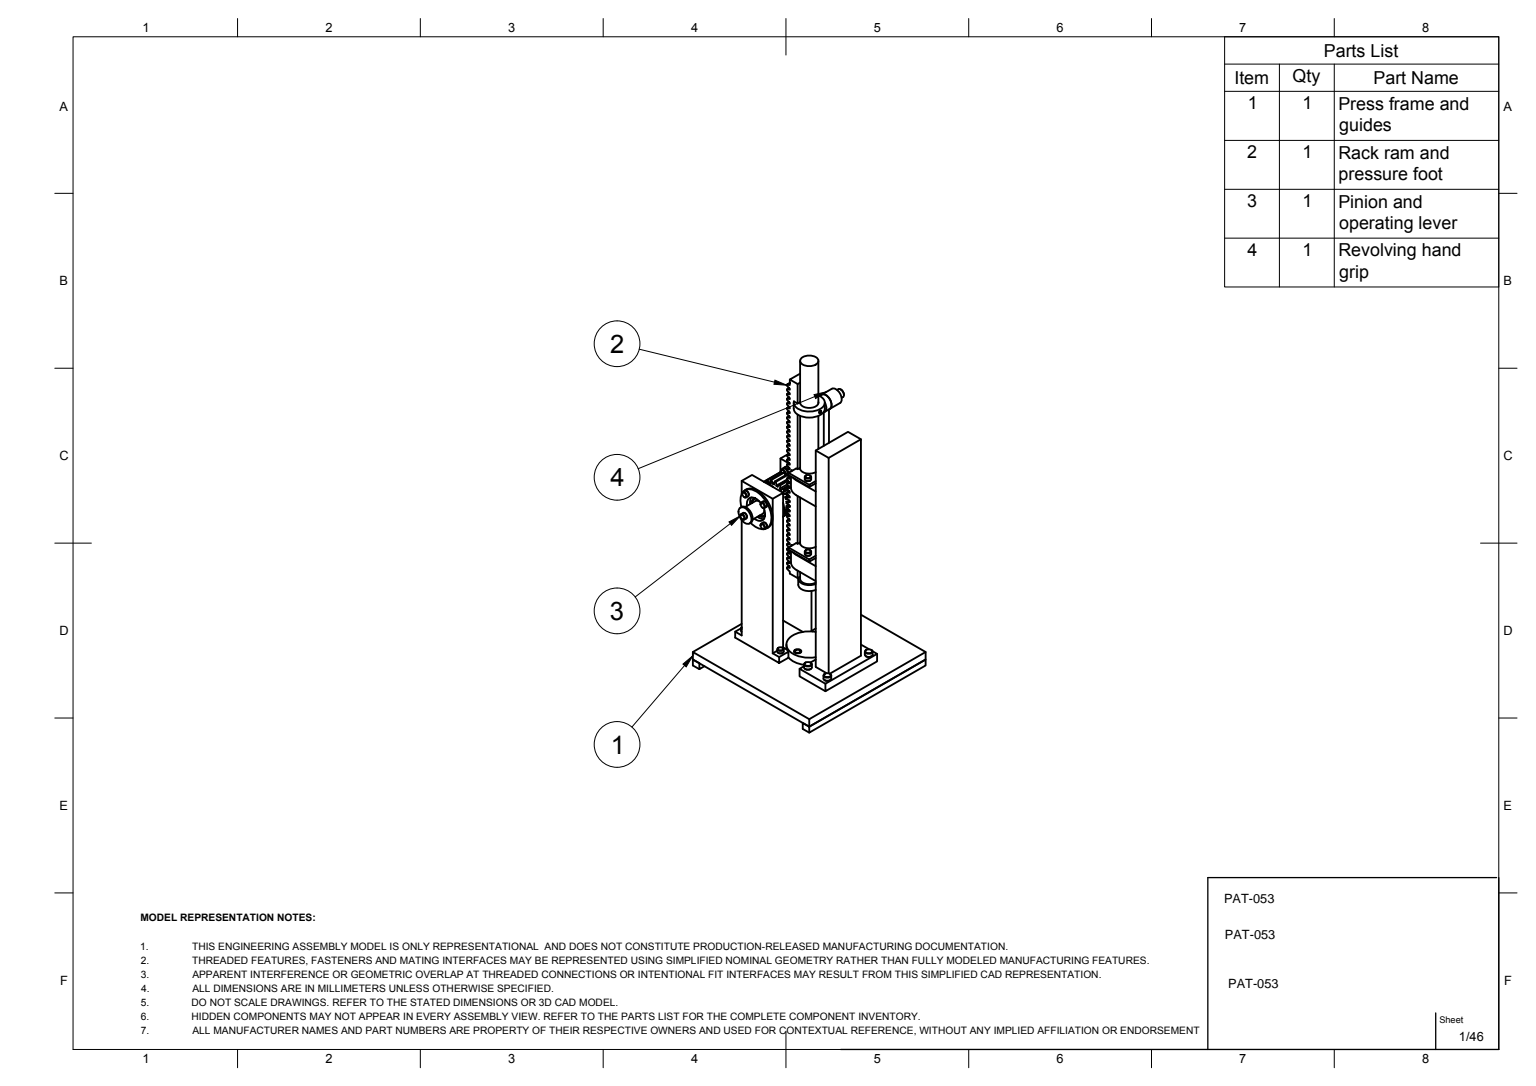
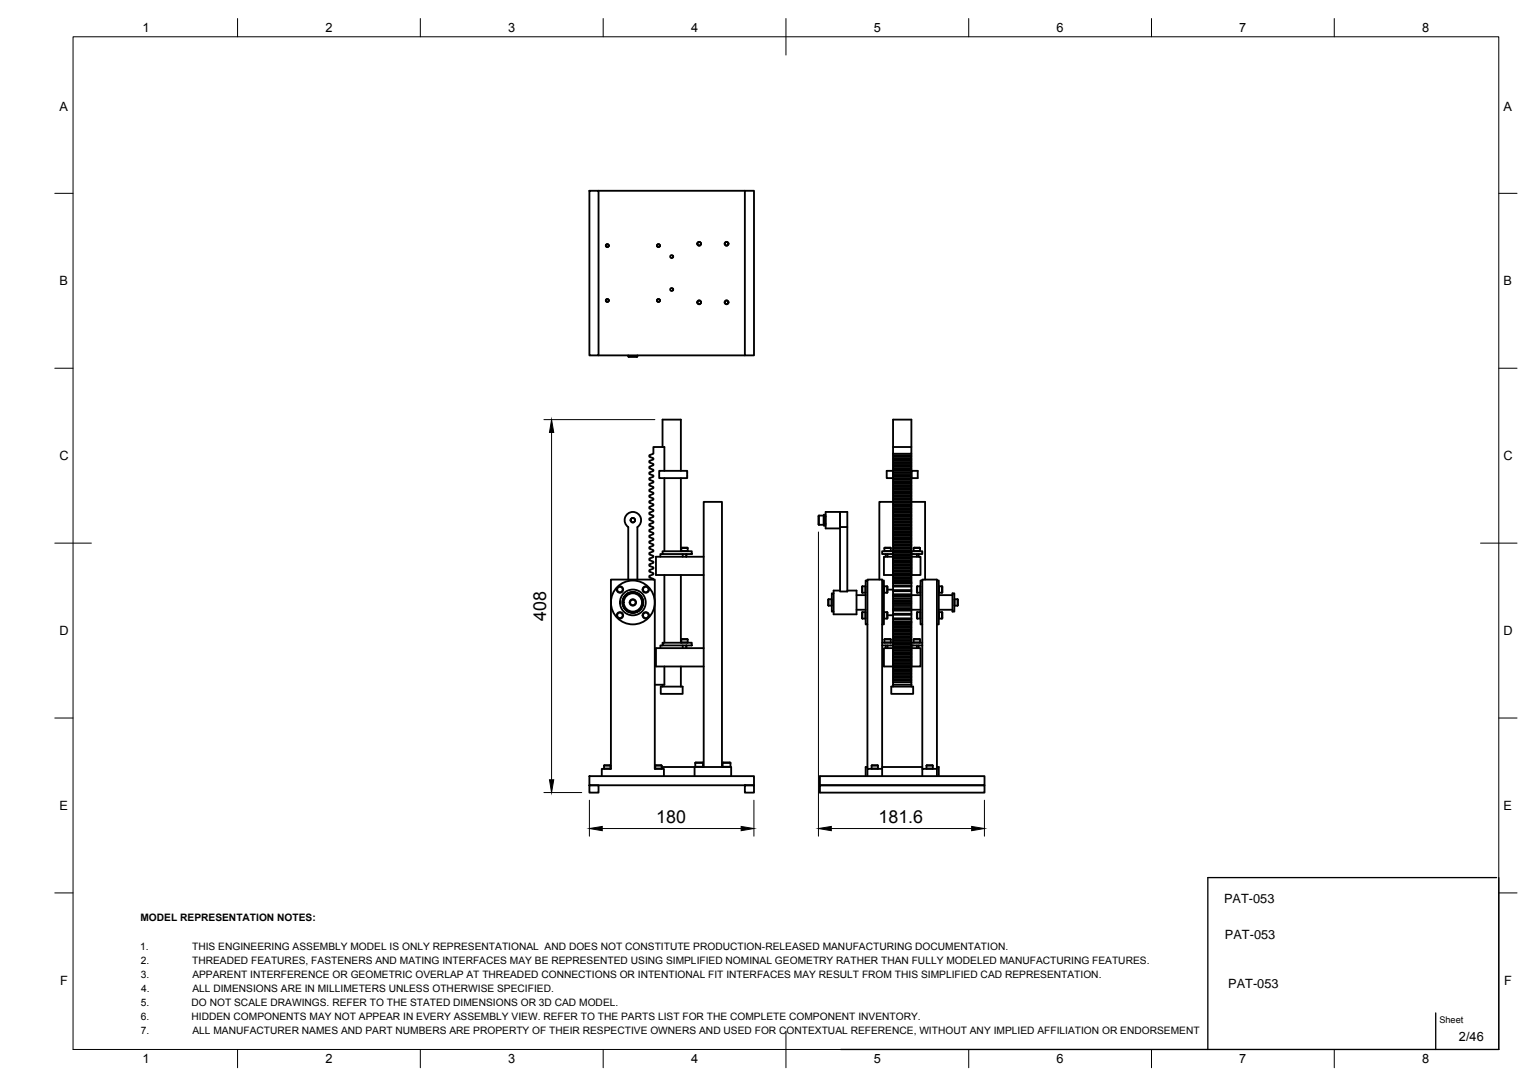
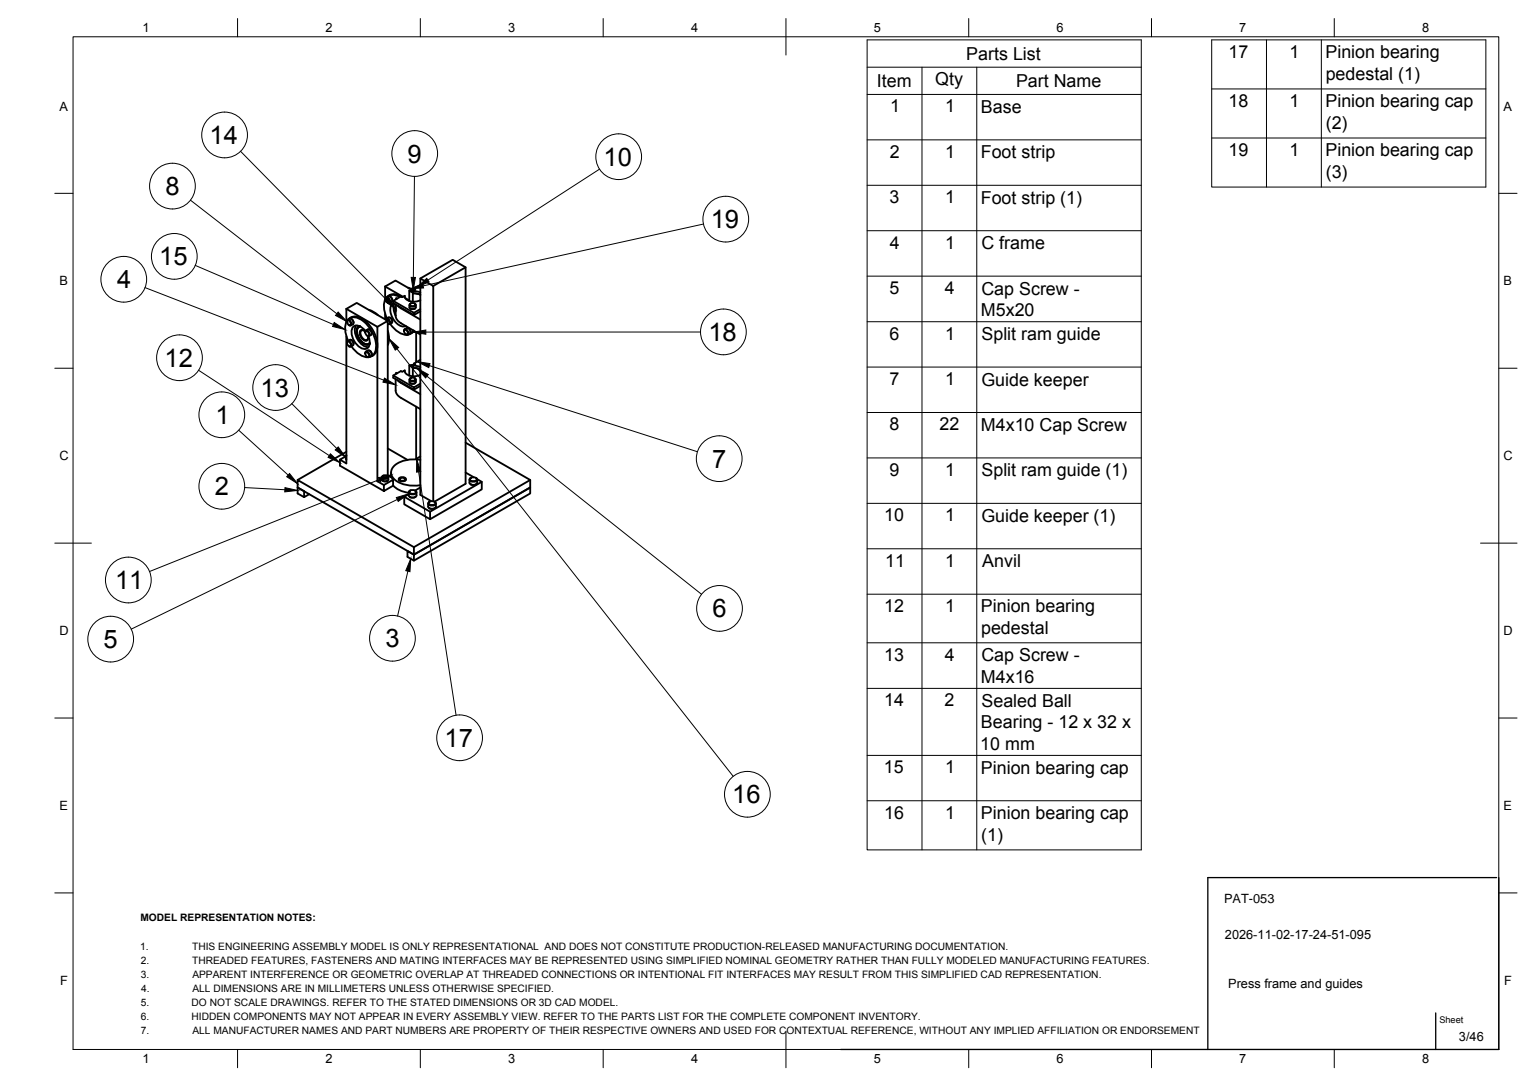
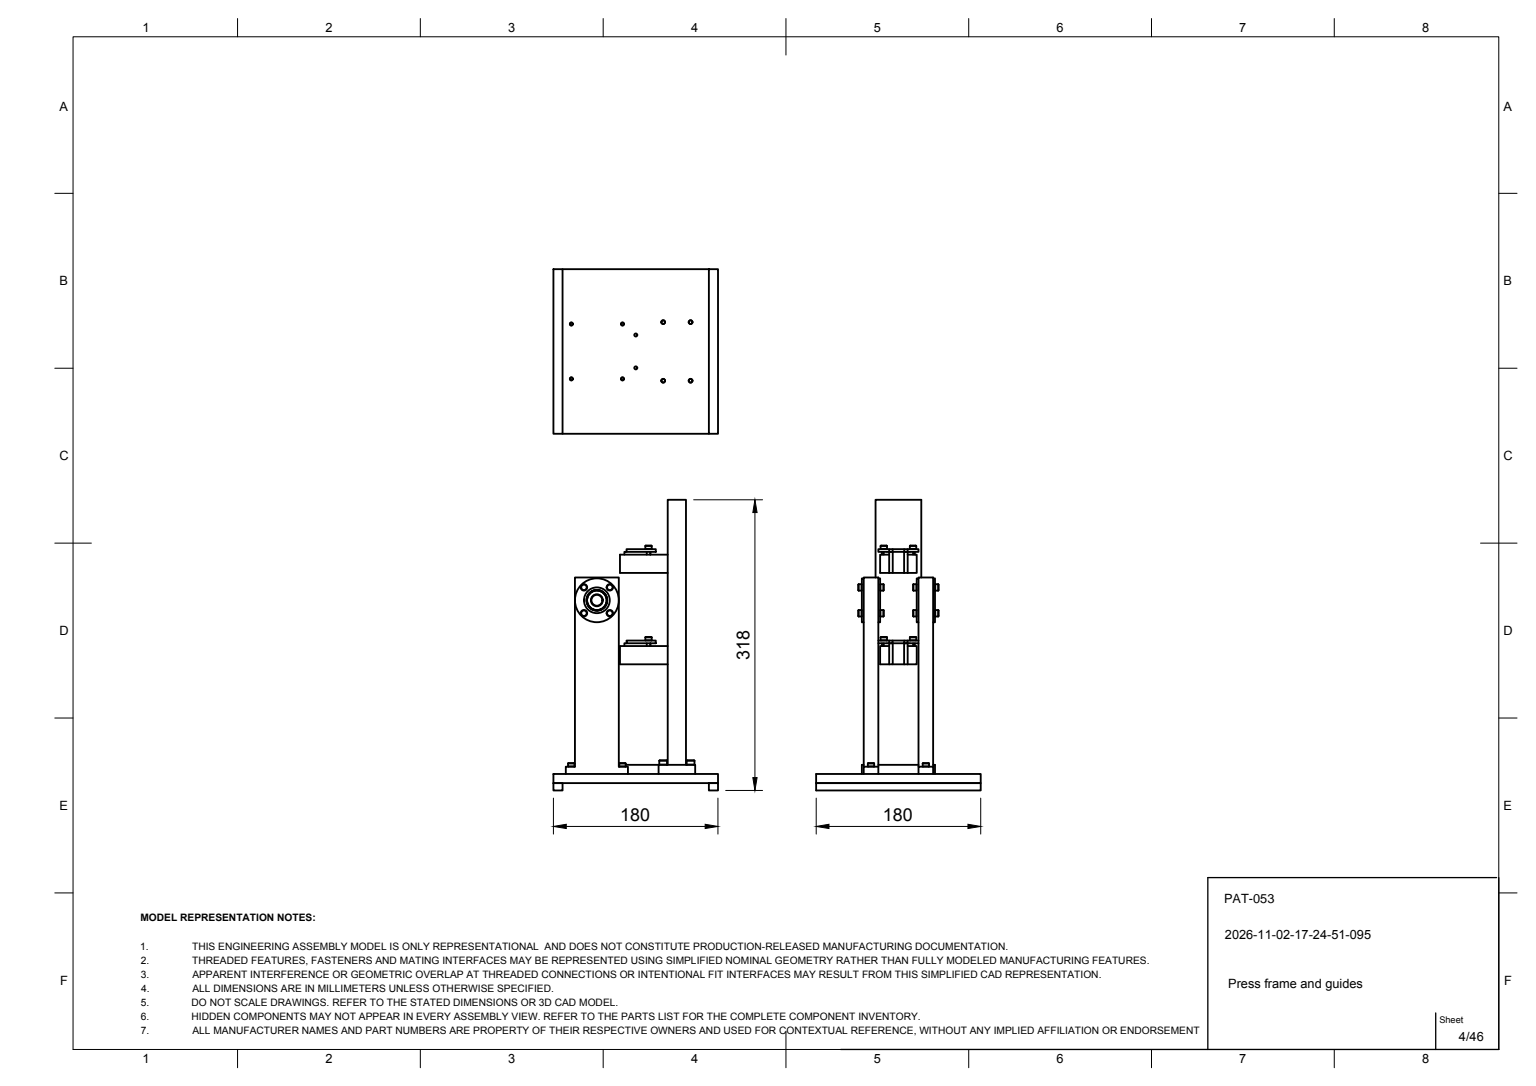
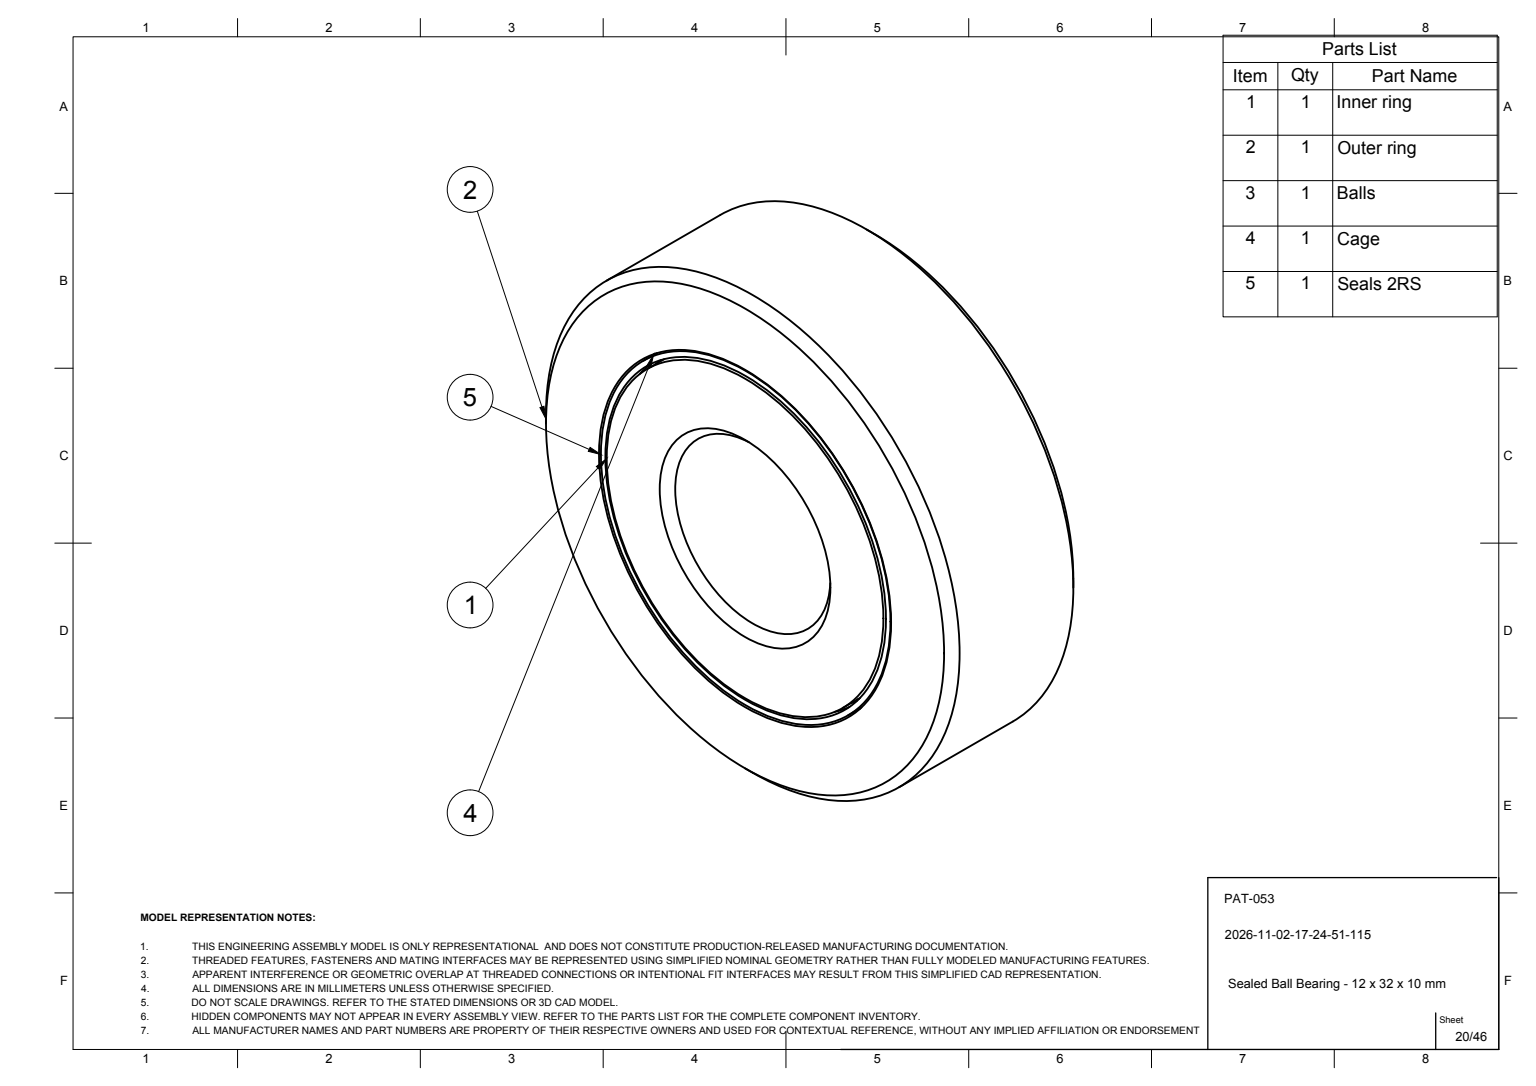
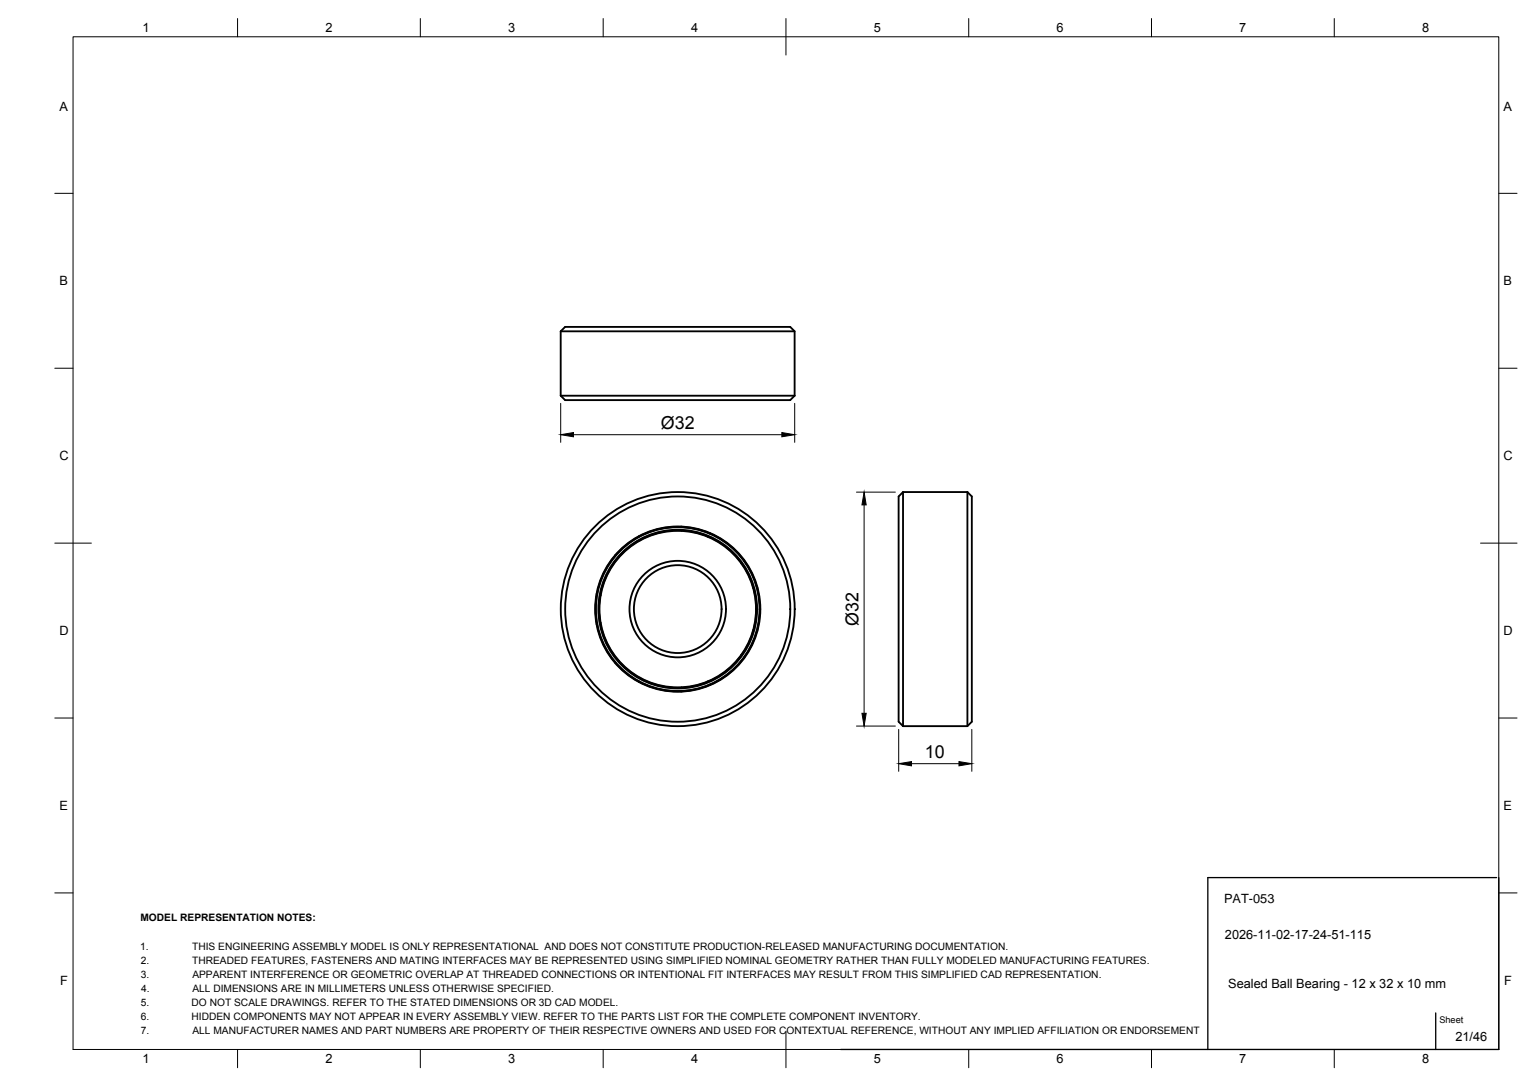
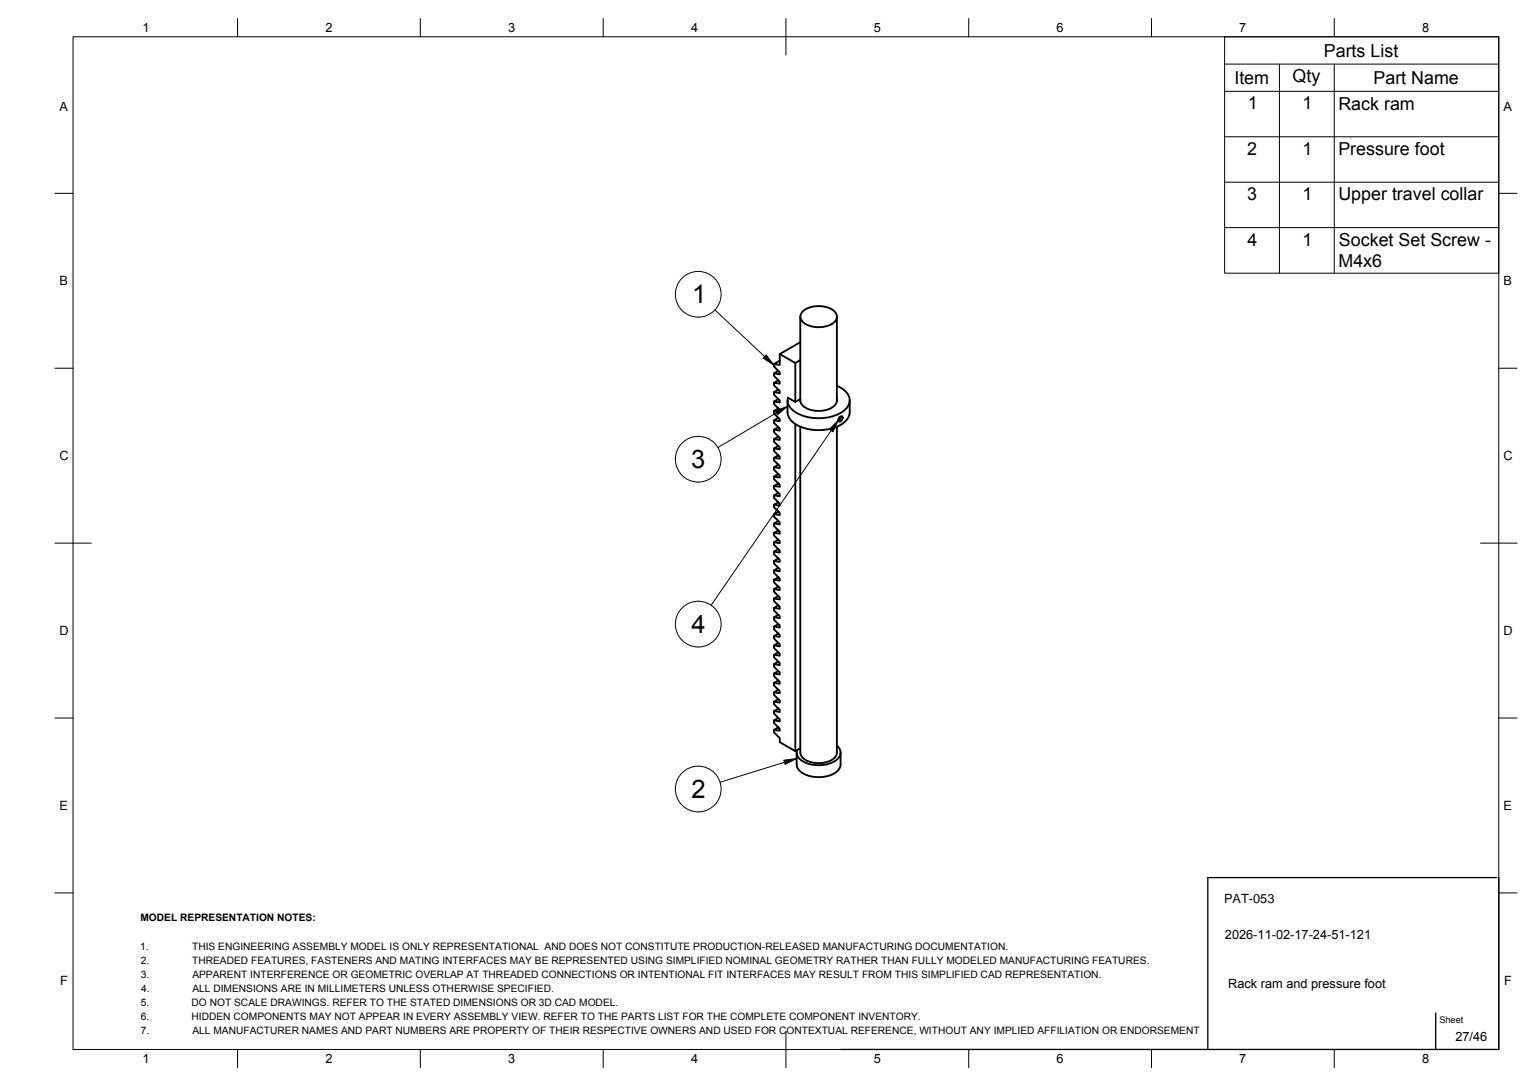
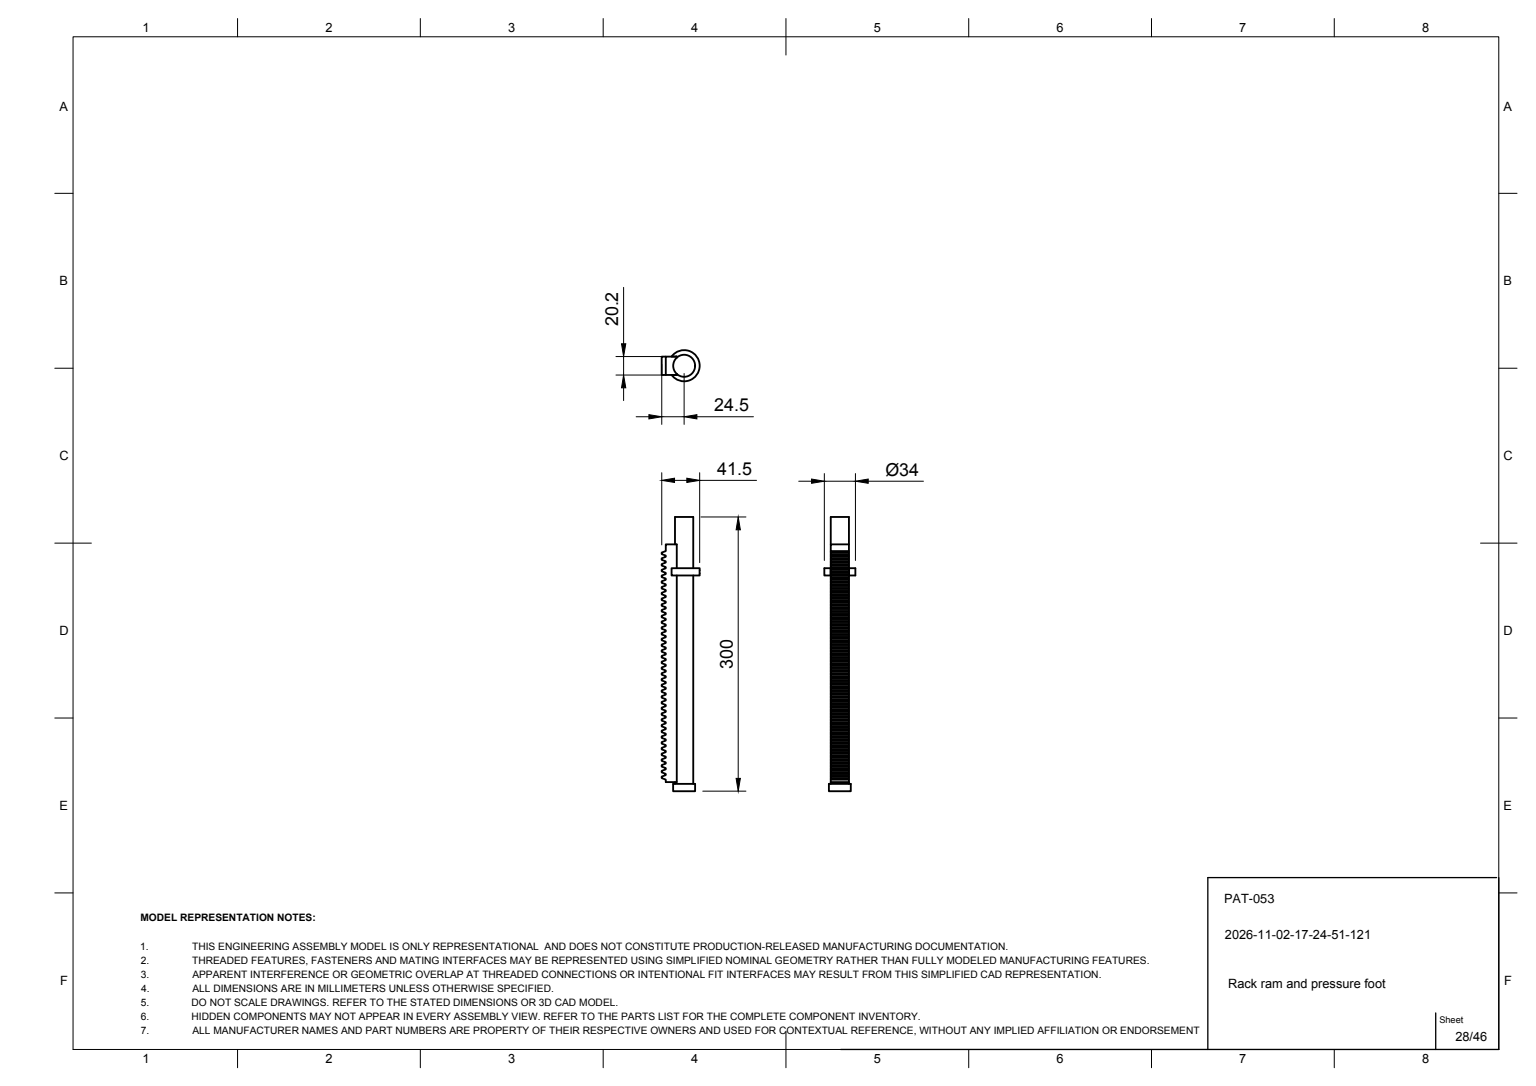
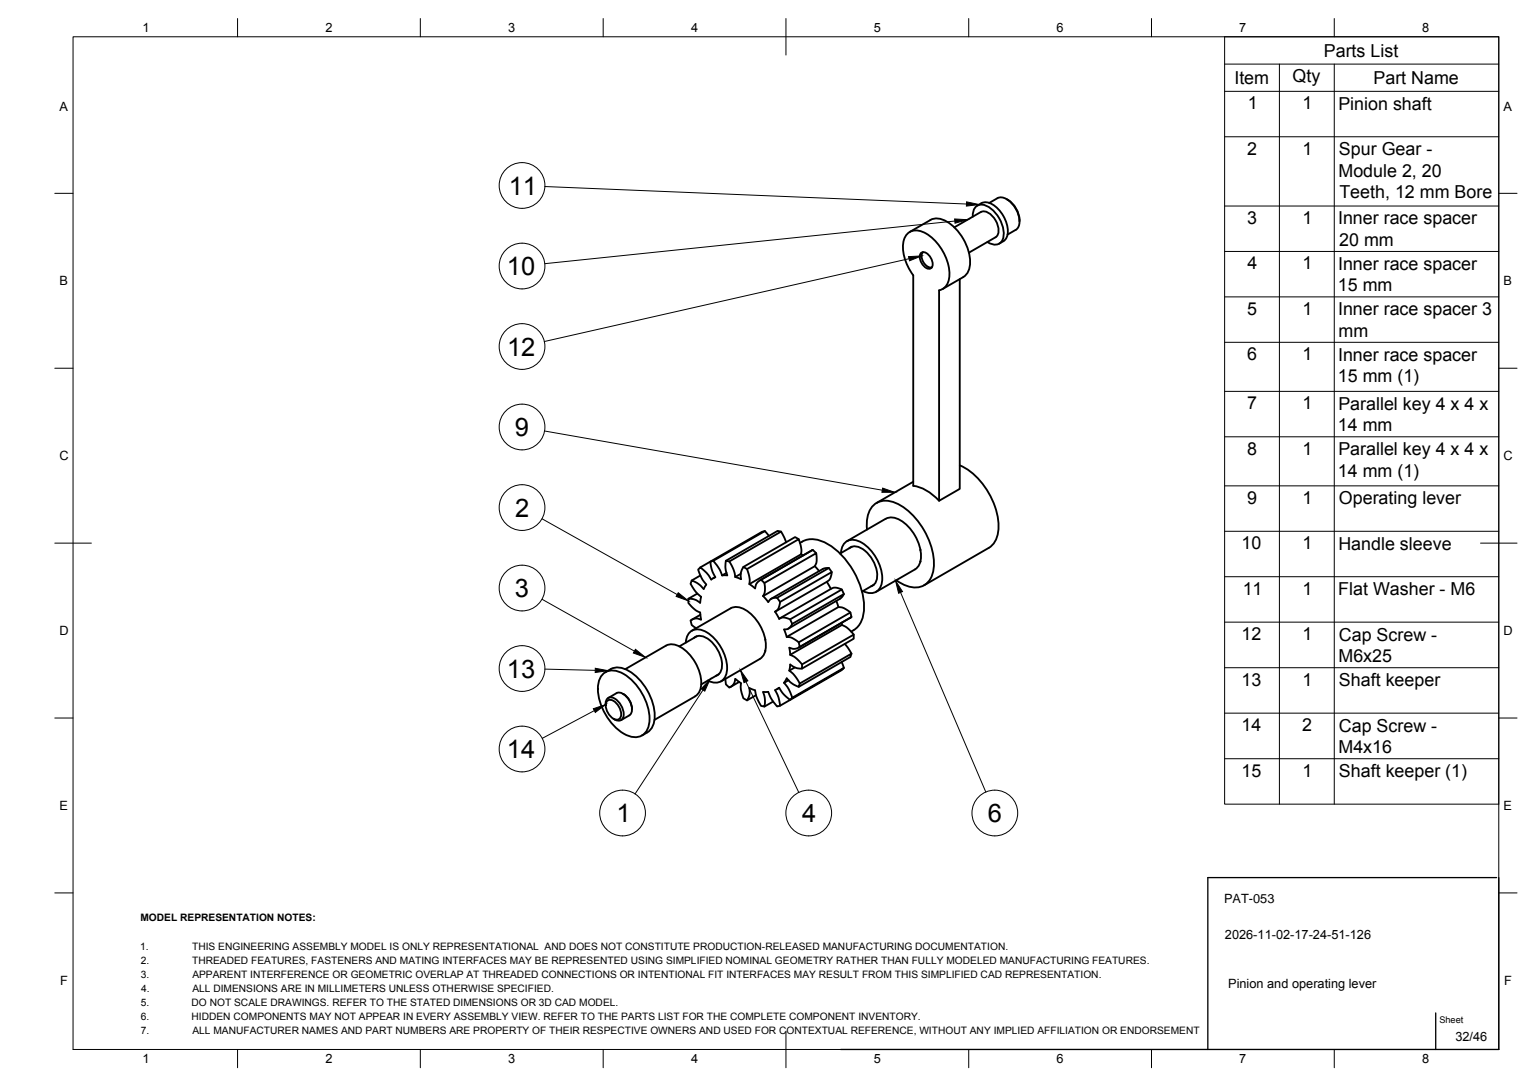
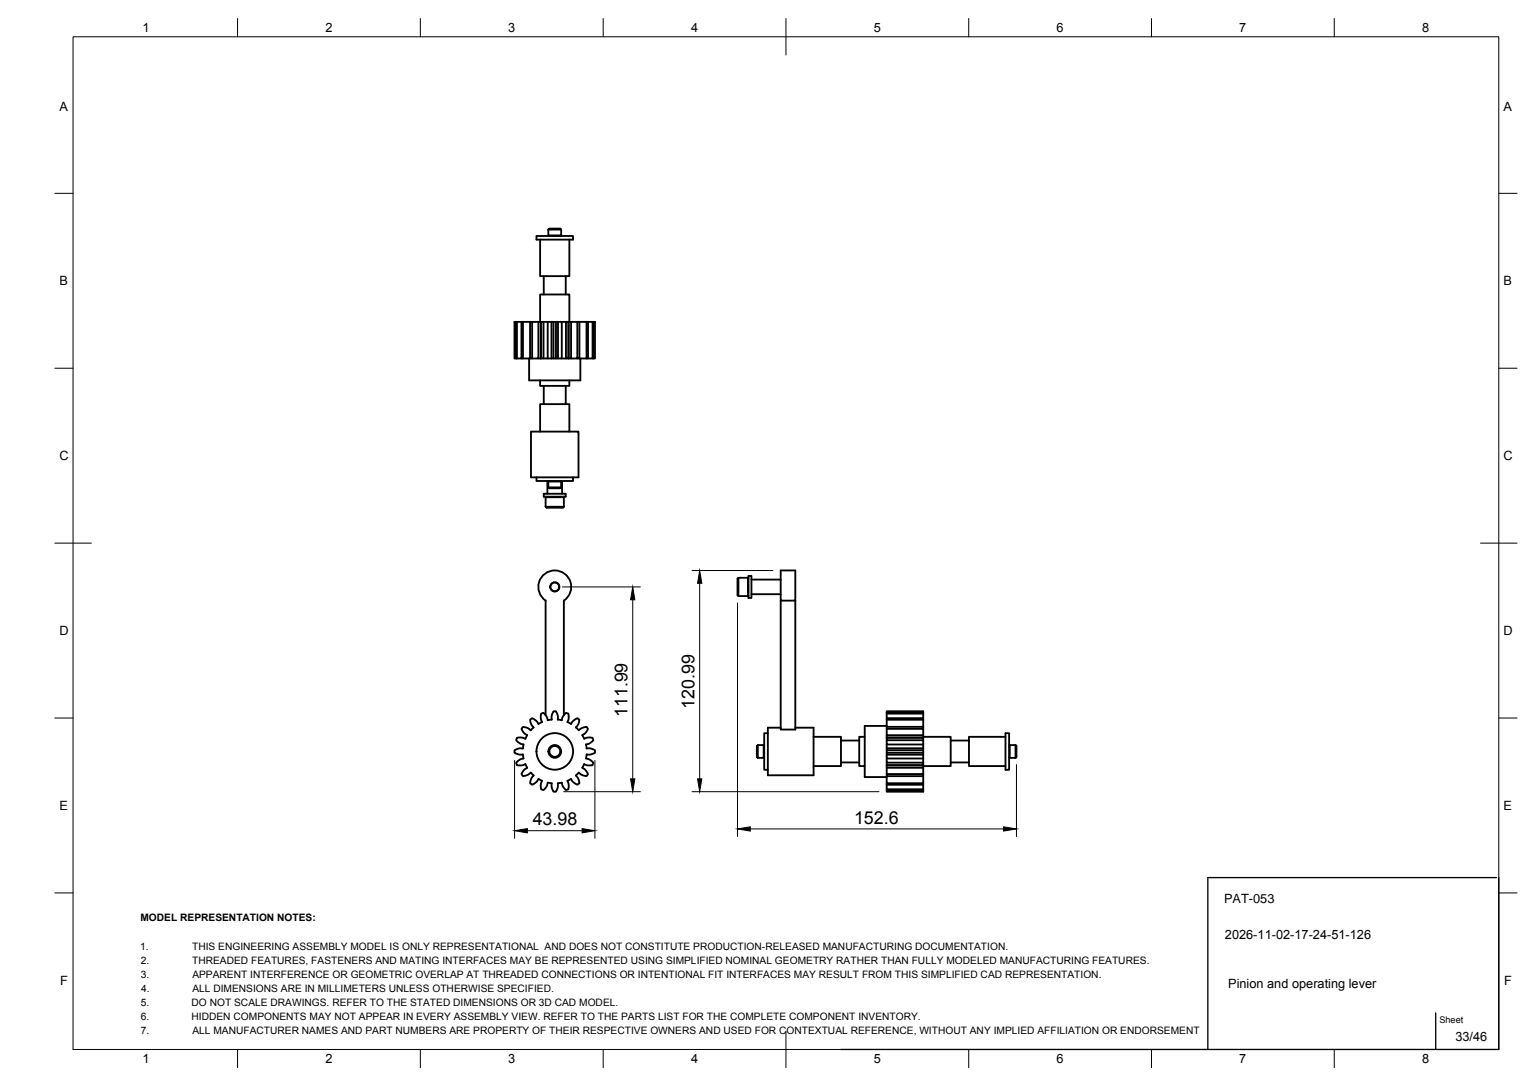
ISO-10303-21;
HEADER;
/* Generated by software containing ST-Developer
 * from STEP Tools, Inc. (www.steptools.com) 
 */

FILE_DESCRIPTION(
/* description */ ('Hand-operated arbor press'),
/* implementation_level */ '2;1');

FILE_NAME(
/* name */ 'PAT-053',
/* time_stamp */ '2026-10-28T03:25:25-07:00',
/* author */ (''),
/* organization */ (''),
/* preprocessor_version */ 'ST-DEVELOPER v20.2',
/* originating_system */ 'Autodesk Translation Framework v15.17.0.0',
/* authorisation */ '');

FILE_SCHEMA (('AUTOMOTIVE_DESIGN { 1 0 10303 214 3 1 1 }'));
ENDSEC;

DATA;
#10=MECHANICAL_DESIGN_GEOMETRIC_PRESENTATION_REPRESENTATION('',(#586,#587,
#588,#589,#590,#591,#592,#593,#594,#595,#596,#597,#598,#599,#600,#601,#602,
#603,#604,#605,#606,#607,#608,#609,#610,#611,#612,#613,#614,#615,#616,#617,
#618,#619,#620,#621,#622,#623,#624,#625,#626,#627,#628,#629,#630,#631,#632,
#633,#634),#32751);
#11=(
BOUNDED_SURFACE()
B_SPLINE_SURFACE(5,1,((#23774,#23775),(#23776,#23777),(#23778,#23779),(#23780,
#23781),(#23782,#23783),(#23784,#23785),(#23786,#23787),(#23788,#23789),
(#23790,#23791),(#23792,#23793),(#23794,#23795),(#23796,#23797),(#23798,
#23799),(#23800,#23801),(#23802,#23803),(#23804,#23805),(#23806,#23807),
(#23808,#23809),(#23810,#23811),(#23812,#23813),(#23814,#23815),(#23816,
#23817),(#23818,#23819),(#23820,#23821),(#23822,#23823),(#23824,#23825),
(#23826,#23827),(#23828,#23829),(#23830,#23831),(#23832,#23833),(#23834,
#23835),(#23836,#23837),(#23838,#23839),(#23840,#23841),(#23842,#23843),
(#23844,#23845),(#23846,#23847),(#23848,#23849),(#23850,#23851),(#23852,
#23853),(#23854,#23855),(#23856,#23857),(#23858,#23859),(#23860,#23861),
(#23862,#23863),(#23864,#23865),(#23866,#23867),(#23868,#23869),(#23870,
#23871),(#23872,#23873),(#23874,#23875),(#23876,#23877),(#23878,#23879),
(#23880,#23881),(#23882,#23883),(#23884,#23885),(#23886,#23887),(#23888,
#23889),(#23890,#23891),(#23892,#23893),(#23894,#23895),(#23896,#23897),
(#23898,#23899),(#23900,#23901),(#23902,#23903),(#23904,#23905),(#23906,
#23907),(#23908,#23909),(#23910,#23911),(#23912,#23913)),.UNSPECIFIED.,
 .F.,.F.,.F.)
B_SPLINE_SURFACE_WITH_KNOTS((6,1,1,1,1,1,1,1,1,1,1,1,1,1,1,1,1,1,1,1,1,
1,1,1,1,1,1,1,1,1,1,1,1,1,1,1,1,1,1,1,1,1,1,1,1,1,1,1,1,1,1,1,1,1,1,1,1,
1,1,1,1,1,1,1,1,6),(2,2),(-1.,-0.984615384615383,-0.969230769230768,-0.953846153846152,
-0.938461538461537,-0.923076923076922,-0.907692307692306,-0.892307692307691,
-0.876923076923076,-0.86153846153846,-0.846153846153845,-0.83076923076923,
-0.815384615384614,-0.799999999999999,-0.784615384615384,-0.769230769230768,
-0.753846153846153,-0.738461538461538,-0.723076923076922,-0.707692307692307,
-0.692307692307692,-0.676923076923076,-0.661538461538461,-0.646153846153846,
-0.63076923076923,-0.615384615384615,-0.6,-0.584615384615384,-0.569230769230769,
-0.553846153846154,-0.538461538461538,-0.523076923076923,-0.507692307692308,
-0.492307692307692,-0.476923076923077,-0.461538461538462,-0.446153846153846,
-0.430769230769231,-0.415384615384615,-0.4,-0.384615384615385,-0.369230769230769,
-0.353846153846154,-0.338461538461538,-0.323076923076923,-0.307692307692308,
-0.292307692307692,-0.276923076923077,-0.261538461538462,-0.246153846153846,
-0.230769230769231,-0.215384615384615,-0.2,-0.184615384615385,-0.169230769230769,
-0.153846153846154,-0.138461538461538,-0.123076923076923,-0.107692307692308,
-0.0923076923076923,-0.0769230769230769,-0.0615384615384615,-0.0461538461538462,
-0.0307692307692308,-0.0153846153846154,0.),(-1.,1.),.UNSPECIFIED.)
GEOMETRIC_REPRESENTATION_ITEM()
RATIONAL_B_SPLINE_SURFACE(((1.,1.),(1.,1.),(1.,1.),(1.,1.),(1.,1.),(1.,
1.),(1.,1.),(1.,1.),(1.,1.),(1.,1.),(1.,1.),(1.,1.),(1.,1.),(1.,1.),(1.,
1.),(1.,1.),(1.,1.),(1.,1.),(1.,1.),(1.,1.),(1.,1.),(1.,1.),(1.,1.),(1.,
1.),(1.,1.),(1.,1.),(1.,1.),(1.,1.),(1.,1.),(1.,1.),(1.,1.),(1.,1.),(1.,
1.),(1.,1.),(1.,1.),(1.,1.),(1.,1.),(1.,1.),(1.,1.),(1.,1.),(1.,1.),(1.,
1.),(1.,1.),(1.,1.),(1.,1.),(1.,1.),(1.,1.),(1.,1.),(1.,1.),(1.,1.),(1.,
1.),(1.,1.),(1.,1.),(1.,1.),(1.,1.),(1.,1.),(1.,1.),(1.,1.),(1.,1.),(1.,
1.),(1.,1.),(1.,1.),(1.,1.),(1.,1.),(1.,1.),(1.,1.),(1.,1.),(1.,1.),(1.,
1.),(1.,1.)))
REPRESENTATION_ITEM('')
SURFACE()
);
#12=(
BOUNDED_SURFACE()
B_SPLINE_SURFACE(5,1,((#23992,#23993),(#23994,#23995),(#23996,#23997),(#23998,
#23999),(#24000,#24001),(#24002,#24003),(#24004,#24005),(#24006,#24007),
(#24008,#24009),(#24010,#24011),(#24012,#24013),(#24014,#24015),(#24016,
#24017),(#24018,#24019),(#24020,#24021),(#24022,#24023),(#24024,#24025),
(#24026,#24027),(#24028,#24029),(#24030,#24031),(#24032,#24033),(#24034,
#24035),(#24036,#24037),(#24038,#24039),(#24040,#24041),(#24042,#24043),
(#24044,#24045),(#24046,#24047),(#24048,#24049),(#24050,#24051),(#24052,
#24053),(#24054,#24055),(#24056,#24057),(#24058,#24059),(#24060,#24061),
(#24062,#24063),(#24064,#24065),(#24066,#24067),(#24068,#24069),(#24070,
#24071),(#24072,#24073),(#24074,#24075),(#24076,#24077),(#24078,#24079),
(#24080,#24081),(#24082,#24083),(#24084,#24085),(#24086,#24087),(#24088,
#24089),(#24090,#24091),(#24092,#24093),(#24094,#24095),(#24096,#24097),
(#24098,#24099),(#24100,#24101),(#24102,#24103),(#24104,#24105),(#24106,
#24107),(#24108,#24109),(#24110,#24111),(#24112,#24113),(#24114,#24115),
(#24116,#24117),(#24118,#24119),(#24120,#24121),(#24122,#24123),(#24124,
#24125),(#24126,#24127),(#24128,#24129),(#24130,#24131)),.UNSPECIFIED.,
 .F.,.F.,.F.)
B_SPLINE_SURFACE_WITH_KNOTS((6,1,1,1,1,1,1,1,1,1,1,1,1,1,1,1,1,1,1,1,1,
1,1,1,1,1,1,1,1,1,1,1,1,1,1,1,1,1,1,1,1,1,1,1,1,1,1,1,1,1,1,1,1,1,1,1,1,
1,1,1,1,1,1,1,1,6),(2,2),(-1.,-0.984615384615383,-0.969230769230768,-0.953846153846152,
-0.938461538461537,-0.923076923076922,-0.907692307692306,-0.892307692307691,
-0.876923076923076,-0.86153846153846,-0.846153846153845,-0.83076923076923,
-0.815384615384614,-0.799999999999999,-0.784615384615384,-0.769230769230768,
-0.753846153846153,-0.738461538461538,-0.723076923076922,-0.707692307692307,
-0.692307692307692,-0.676923076923076,-0.661538461538461,-0.646153846153846,
-0.63076923076923,-0.615384615384615,-0.6,-0.584615384615384,-0.569230769230769,
-0.553846153846154,-0.538461538461538,-0.523076923076923,-0.507692307692308,
-0.492307692307692,-0.476923076923077,-0.461538461538462,-0.446153846153846,
-0.430769230769231,-0.415384615384615,-0.4,-0.384615384615385,-0.369230769230769,
-0.353846153846154,-0.338461538461538,-0.323076923076923,-0.307692307692308,
-0.292307692307692,-0.276923076923077,-0.261538461538462,-0.246153846153846,
-0.230769230769231,-0.215384615384615,-0.2,-0.184615384615385,-0.169230769230769,
-0.153846153846154,-0.138461538461538,-0.123076923076923,-0.107692307692308,
-0.0923076923076923,-0.0769230769230769,-0.0615384615384615,-0.0461538461538462,
-0.0307692307692308,-0.0153846153846154,0.),(-1.,1.),.UNSPECIFIED.)
GEOMETRIC_REPRESENTATION_ITEM()
RATIONAL_B_SPLINE_SURFACE(((1.,1.),(1.,1.),(1.,1.),(1.,1.),(1.,1.),(1.,
1.),(1.,1.),(1.,1.),(1.,1.),(1.,1.),(1.,1.),(1.,1.),(1.,1.),(1.,1.),(1.,
1.),(1.,1.),(1.,1.),(1.,1.),(1.,1.),(1.,1.),(1.,1.),(1.,1.),(1.,1.),(1.,
1.),(1.,1.),(1.,1.),(1.,1.),(1.,1.),(1.,1.),(1.,1.),(1.,1.),(1.,1.),(1.,
1.),(1.,1.),(1.,1.),(1.,1.),(1.,1.),(1.,1.),(1.,1.),(1.,1.),(1.,1.),(1.,
1.),(1.,1.),(1.,1.),(1.,1.),(1.,1.),(1.,1.),(1.,1.),(1.,1.),(1.,1.),(1.,
1.),(1.,1.),(1.,1.),(1.,1.),(1.,1.),(1.,1.),(1.,1.),(1.,1.),(1.,1.),(1.,
1.),(1.,1.),(1.,1.),(1.,1.),(1.,1.),(1.,1.),(1.,1.),(1.,1.),(1.,1.),(1.,
1.),(1.,1.)))
REPRESENTATION_ITEM('')
SURFACE()
);
#13=(
BOUNDED_SURFACE()
B_SPLINE_SURFACE(5,1,((#24208,#24209),(#24210,#24211),(#24212,#24213),(#24214,
#24215),(#24216,#24217),(#24218,#24219),(#24220,#24221),(#24222,#24223),
(#24224,#24225),(#24226,#24227),(#24228,#24229),(#24230,#24231),(#24232,
#24233),(#24234,#24235),(#24236,#24237),(#24238,#24239),(#24240,#24241),
(#24242,#24243),(#24244,#24245),(#24246,#24247),(#24248,#24249),(#24250,
#24251),(#24252,#24253),(#24254,#24255),(#24256,#24257),(#24258,#24259),
(#24260,#24261),(#24262,#24263),(#24264,#24265),(#24266,#24267),(#24268,
#24269),(#24270,#24271),(#24272,#24273),(#24274,#24275),(#24276,#24277),
(#24278,#24279),(#24280,#24281),(#24282,#24283),(#24284,#24285),(#24286,
#24287),(#24288,#24289),(#24290,#24291),(#24292,#24293),(#24294,#24295),
(#24296,#24297),(#24298,#24299),(#24300,#24301),(#24302,#24303),(#24304,
#24305),(#24306,#24307),(#24308,#24309),(#24310,#24311),(#24312,#24313),
(#24314,#24315),(#24316,#24317),(#24318,#24319),(#24320,#24321),(#24322,
#24323),(#24324,#24325),(#24326,#24327),(#24328,#24329),(#24330,#24331),
(#24332,#24333),(#24334,#24335),(#24336,#24337),(#24338,#24339),(#24340,
#24341),(#24342,#24343),(#24344,#24345),(#24346,#24347)),.UNSPECIFIED.,
 .F.,.F.,.F.)
B_SPLINE_SURFACE_WITH_KNOTS((6,1,1,1,1,1,1,1,1,1,1,1,1,1,1,1,1,1,1,1,1,
1,1,1,1,1,1,1,1,1,1,1,1,1,1,1,1,1,1,1,1,1,1,1,1,1,1,1,1,1,1,1,1,1,1,1,1,
1,1,1,1,1,1,1,1,6),(2,2),(-1.,-0.984615384615383,-0.969230769230768,-0.953846153846152,
-0.938461538461537,-0.923076923076922,-0.907692307692306,-0.892307692307691,
-0.876923076923076,-0.86153846153846,-0.846153846153845,-0.83076923076923,
-0.815384615384614,-0.799999999999999,-0.784615384615384,-0.769230769230768,
-0.753846153846153,-0.738461538461538,-0.723076923076922,-0.707692307692307,
-0.692307692307692,-0.676923076923076,-0.661538461538461,-0.646153846153846,
-0.63076923076923,-0.615384615384615,-0.6,-0.584615384615384,-0.569230769230769,
-0.553846153846154,-0.538461538461538,-0.523076923076923,-0.507692307692308,
-0.492307692307692,-0.476923076923077,-0.461538461538462,-0.446153846153846,
-0.430769230769231,-0.415384615384615,-0.4,-0.384615384615385,-0.369230769230769,
-0.353846153846154,-0.338461538461538,-0.323076923076923,-0.307692307692308,
-0.292307692307692,-0.276923076923077,-0.261538461538462,-0.246153846153846,
-0.230769230769231,-0.215384615384615,-0.2,-0.184615384615385,-0.169230769230769,
-0.153846153846154,-0.138461538461538,-0.123076923076923,-0.107692307692308,
-0.0923076923076923,-0.0769230769230769,-0.0615384615384615,-0.0461538461538462,
-0.0307692307692308,-0.0153846153846154,0.),(-1.,1.),.UNSPECIFIED.)
GEOMETRIC_REPRESENTATION_ITEM()
RATIONAL_B_SPLINE_SURFACE(((1.,1.),(1.,1.),(1.,1.),(1.,1.),(1.,1.),(1.,
1.),(1.,1.),(1.,1.),(1.,1.),(1.,1.),(1.,1.),(1.,1.),(1.,1.),(1.,1.),(1.,
1.),(1.,1.),(1.,1.),(1.,1.),(1.,1.),(1.,1.),(1.,1.),(1.,1.),(1.,1.),(1.,
1.),(1.,1.),(1.,1.),(1.,1.),(1.,1.),(1.,1.),(1.,1.),(1.,1.),(1.,1.),(1.,
1.),(1.,1.),(1.,1.),(1.,1.),(1.,1.),(1.,1.),(1.,1.),(1.,1.),(1.,1.),(1.,
1.),(1.,1.),(1.,1.),(1.,1.),(1.,1.),(1.,1.),(1.,1.),(1.,1.),(1.,1.),(1.,
1.),(1.,1.),(1.,1.),(1.,1.),(1.,1.),(1.,1.),(1.,1.),(1.,1.),(1.,1.),(1.,
1.),(1.,1.),(1.,1.),(1.,1.),(1.,1.),(1.,1.),(1.,1.),(1.,1.),(1.,1.),(1.,
1.),(1.,1.)))
REPRESENTATION_ITEM('')
SURFACE()
);
#14=(
BOUNDED_SURFACE()
B_SPLINE_SURFACE(5,1,((#24424,#24425),(#24426,#24427),(#24428,#24429),(#24430,
#24431),(#24432,#24433),(#24434,#24435),(#24436,#24437),(#24438,#24439),
(#24440,#24441),(#24442,#24443),(#24444,#24445),(#24446,#24447),(#24448,
#24449),(#24450,#24451),(#24452,#24453),(#24454,#24455),(#24456,#24457),
(#24458,#24459),(#24460,#24461),(#24462,#24463),(#24464,#24465),(#24466,
#24467),(#24468,#24469),(#24470,#24471),(#24472,#24473),(#24474,#24475),
(#24476,#24477),(#24478,#24479),(#24480,#24481),(#24482,#24483),(#24484,
#24485),(#24486,#24487),(#24488,#24489),(#24490,#24491),(#24492,#24493),
(#24494,#24495),(#24496,#24497),(#24498,#24499),(#24500,#24501),(#24502,
#24503),(#24504,#24505),(#24506,#24507),(#24508,#24509),(#24510,#24511),
(#24512,#24513),(#24514,#24515),(#24516,#24517),(#24518,#24519),(#24520,
#24521),(#24522,#24523),(#24524,#24525),(#24526,#24527),(#24528,#24529),
(#24530,#24531),(#24532,#24533),(#24534,#24535),(#24536,#24537),(#24538,
#24539),(#24540,#24541),(#24542,#24543),(#24544,#24545),(#24546,#24547),
(#24548,#24549),(#24550,#24551),(#24552,#24553),(#24554,#24555),(#24556,
#24557),(#24558,#24559),(#24560,#24561),(#24562,#24563)),.UNSPECIFIED.,
 .F.,.F.,.F.)
B_SPLINE_SURFACE_WITH_KNOTS((6,1,1,1,1,1,1,1,1,1,1,1,1,1,1,1,1,1,1,1,1,
1,1,1,1,1,1,1,1,1,1,1,1,1,1,1,1,1,1,1,1,1,1,1,1,1,1,1,1,1,1,1,1,1,1,1,1,
1,1,1,1,1,1,1,1,6),(2,2),(-1.,-0.984615384615383,-0.969230769230768,-0.953846153846152,
-0.938461538461537,-0.923076923076922,-0.907692307692306,-0.892307692307691,
-0.876923076923076,-0.86153846153846,-0.846153846153845,-0.83076923076923,
-0.815384615384614,-0.799999999999999,-0.784615384615384,-0.769230769230768,
-0.753846153846153,-0.738461538461538,-0.723076923076922,-0.707692307692307,
-0.692307692307692,-0.676923076923076,-0.661538461538461,-0.646153846153846,
-0.63076923076923,-0.615384615384615,-0.6,-0.584615384615384,-0.569230769230769,
-0.553846153846154,-0.538461538461538,-0.523076923076923,-0.507692307692308,
-0.492307692307692,-0.476923076923077,-0.461538461538462,-0.446153846153846,
-0.430769230769231,-0.415384615384615,-0.4,-0.384615384615385,-0.369230769230769,
-0.353846153846154,-0.338461538461538,-0.323076923076923,-0.307692307692308,
-0.292307692307692,-0.276923076923077,-0.261538461538462,-0.246153846153846,
-0.230769230769231,-0.215384615384615,-0.2,-0.184615384615385,-0.169230769230769,
-0.153846153846154,-0.138461538461538,-0.123076923076923,-0.107692307692308,
-0.0923076923076923,-0.0769230769230769,-0.0615384615384615,-0.0461538461538462,
-0.0307692307692308,-0.0153846153846154,0.),(-1.,1.),.UNSPECIFIED.)
GEOMETRIC_REPRESENTATION_ITEM()
RATIONAL_B_SPLINE_SURFACE(((1.,1.),(1.,1.),(1.,1.),(1.,1.),(1.,1.),(1.,
1.),(1.,1.),(1.,1.),(1.,1.),(1.,1.),(1.,1.),(1.,1.),(1.,1.),(1.,1.),(1.,
1.),(1.,1.),(1.,1.),(1.,1.),(1.,1.),(1.,1.),(1.,1.),(1.,1.),(1.,1.),(1.,
1.),(1.,1.),(1.,1.),(1.,1.),(1.,1.),(1.,1.),(1.,1.),(1.,1.),(1.,1.),(1.,
1.),(1.,1.),(1.,1.),(1.,1.),(1.,1.),(1.,1.),(1.,1.),(1.,1.),(1.,1.),(1.,
1.),(1.,1.),(1.,1.),(1.,1.),(1.,1.),(1.,1.),(1.,1.),(1.,1.),(1.,1.),(1.,
1.),(1.,1.),(1.,1.),(1.,1.),(1.,1.),(1.,1.),(1.,1.),(1.,1.),(1.,1.),(1.,
1.),(1.,1.),(1.,1.),(1.,1.),(1.,1.),(1.,1.),(1.,1.),(1.,1.),(1.,1.),(1.,
1.),(1.,1.)))
REPRESENTATION_ITEM('')
SURFACE()
);
#15=(
BOUNDED_SURFACE()
B_SPLINE_SURFACE(5,1,((#24640,#24641),(#24642,#24643),(#24644,#24645),(#24646,
#24647),(#24648,#24649),(#24650,#24651),(#24652,#24653),(#24654,#24655),
(#24656,#24657),(#24658,#24659),(#24660,#24661),(#24662,#24663),(#24664,
#24665),(#24666,#24667),(#24668,#24669),(#24670,#24671),(#24672,#24673),
(#24674,#24675),(#24676,#24677),(#24678,#24679),(#24680,#24681),(#24682,
#24683),(#24684,#24685),(#24686,#24687),(#24688,#24689),(#24690,#24691),
(#24692,#24693),(#24694,#24695),(#24696,#24697),(#24698,#24699),(#24700,
#24701),(#24702,#24703),(#24704,#24705),(#24706,#24707),(#24708,#24709),
(#24710,#24711),(#24712,#24713),(#24714,#24715),(#24716,#24717),(#24718,
#24719),(#24720,#24721),(#24722,#24723),(#24724,#24725),(#24726,#24727),
(#24728,#24729),(#24730,#24731),(#24732,#24733),(#24734,#24735),(#24736,
#24737),(#24738,#24739),(#24740,#24741),(#24742,#24743),(#24744,#24745),
(#24746,#24747),(#24748,#24749),(#24750,#24751),(#24752,#24753),(#24754,
#24755),(#24756,#24757),(#24758,#24759),(#24760,#24761),(#24762,#24763),
(#24764,#24765),(#24766,#24767),(#24768,#24769),(#24770,#24771),(#24772,
#24773),(#24774,#24775),(#24776,#24777),(#24778,#24779)),.UNSPECIFIED.,
 .F.,.F.,.F.)
B_SPLINE_SURFACE_WITH_KNOTS((6,1,1,1,1,1,1,1,1,1,1,1,1,1,1,1,1,1,1,1,1,
1,1,1,1,1,1,1,1,1,1,1,1,1,1,1,1,1,1,1,1,1,1,1,1,1,1,1,1,1,1,1,1,1,1,1,1,
1,1,1,1,1,1,1,1,6),(2,2),(-1.,-0.984615384615383,-0.969230769230768,-0.953846153846152,
-0.938461538461537,-0.923076923076922,-0.907692307692306,-0.892307692307691,
-0.876923076923076,-0.86153846153846,-0.846153846153845,-0.83076923076923,
-0.815384615384614,-0.799999999999999,-0.784615384615384,-0.769230769230768,
-0.753846153846153,-0.738461538461538,-0.723076923076922,-0.707692307692307,
-0.692307692307692,-0.676923076923076,-0.661538461538461,-0.646153846153846,
-0.63076923076923,-0.615384615384615,-0.6,-0.584615384615384,-0.569230769230769,
-0.553846153846154,-0.538461538461538,-0.523076923076923,-0.507692307692308,
-0.492307692307692,-0.476923076923077,-0.461538461538462,-0.446153846153846,
-0.430769230769231,-0.415384615384615,-0.4,-0.384615384615385,-0.369230769230769,
-0.353846153846154,-0.338461538461538,-0.323076923076923,-0.307692307692308,
-0.292307692307692,-0.276923076923077,-0.261538461538462,-0.246153846153846,
-0.230769230769231,-0.215384615384615,-0.2,-0.184615384615385,-0.169230769230769,
-0.153846153846154,-0.138461538461538,-0.123076923076923,-0.107692307692308,
-0.0923076923076923,-0.0769230769230769,-0.0615384615384615,-0.0461538461538462,
-0.0307692307692308,-0.0153846153846154,0.),(-1.,1.),.UNSPECIFIED.)
GEOMETRIC_REPRESENTATION_ITEM()
RATIONAL_B_SPLINE_SURFACE(((1.,1.),(1.,1.),(1.,1.),(1.,1.),(1.,1.),(1.,
1.),(1.,1.),(1.,1.),(1.,1.),(1.,1.),(1.,1.),(1.,1.),(1.,1.),(1.,1.),(1.,
1.),(1.,1.),(1.,1.),(1.,1.),(1.,1.),(1.,1.),(1.,1.),(1.,1.),(1.,1.),(1.,
1.),(1.,1.),(1.,1.),(1.,1.),(1.,1.),(1.,1.),(1.,1.),(1.,1.),(1.,1.),(1.,
1.),(1.,1.),(1.,1.),(1.,1.),(1.,1.),(1.,1.),(1.,1.),(1.,1.),(1.,1.),(1.,
1.),(1.,1.),(1.,1.),(1.,1.),(1.,1.),(1.,1.),(1.,1.),(1.,1.),(1.,1.),(1.,
1.),(1.,1.),(1.,1.),(1.,1.),(1.,1.),(1.,1.),(1.,1.),(1.,1.),(1.,1.),(1.,
1.),(1.,1.),(1.,1.),(1.,1.),(1.,1.),(1.,1.),(1.,1.),(1.,1.),(1.,1.),(1.,
1.),(1.,1.)))
REPRESENTATION_ITEM('')
SURFACE()
);
#16=(
BOUNDED_SURFACE()
B_SPLINE_SURFACE(5,1,((#24856,#24857),(#24858,#24859),(#24860,#24861),(#24862,
#24863),(#24864,#24865),(#24866,#24867),(#24868,#24869),(#24870,#24871),
(#24872,#24873),(#24874,#24875),(#24876,#24877),(#24878,#24879),(#24880,
#24881),(#24882,#24883),(#24884,#24885),(#24886,#24887),(#24888,#24889),
(#24890,#24891),(#24892,#24893),(#24894,#24895),(#24896,#24897),(#24898,
#24899),(#24900,#24901),(#24902,#24903),(#24904,#24905),(#24906,#24907),
(#24908,#24909),(#24910,#24911),(#24912,#24913),(#24914,#24915),(#24916,
#24917),(#24918,#24919),(#24920,#24921),(#24922,#24923),(#24924,#24925),
(#24926,#24927),(#24928,#24929),(#24930,#24931),(#24932,#24933),(#24934,
#24935),(#24936,#24937),(#24938,#24939),(#24940,#24941),(#24942,#24943),
(#24944,#24945),(#24946,#24947),(#24948,#24949),(#24950,#24951),(#24952,
#24953),(#24954,#24955),(#24956,#24957),(#24958,#24959),(#24960,#24961),
(#24962,#24963),(#24964,#24965),(#24966,#24967),(#24968,#24969),(#24970,
#24971),(#24972,#24973),(#24974,#24975),(#24976,#24977),(#24978,#24979),
(#24980,#24981),(#24982,#24983),(#24984,#24985),(#24986,#24987),(#24988,
#24989),(#24990,#24991),(#24992,#24993),(#24994,#24995)),.UNSPECIFIED.,
 .F.,.F.,.F.)
B_SPLINE_SURFACE_WITH_KNOTS((6,1,1,1,1,1,1,1,1,1,1,1,1,1,1,1,1,1,1,1,1,
1,1,1,1,1,1,1,1,1,1,1,1,1,1,1,1,1,1,1,1,1,1,1,1,1,1,1,1,1,1,1,1,1,1,1,1,
1,1,1,1,1,1,1,1,6),(2,2),(-1.,-0.984615384615383,-0.969230769230768,-0.953846153846152,
-0.938461538461537,-0.923076923076922,-0.907692307692306,-0.892307692307691,
-0.876923076923076,-0.86153846153846,-0.846153846153845,-0.83076923076923,
-0.815384615384614,-0.799999999999999,-0.784615384615384,-0.769230769230768,
-0.753846153846153,-0.738461538461538,-0.723076923076922,-0.707692307692307,
-0.692307692307692,-0.676923076923076,-0.661538461538461,-0.646153846153846,
-0.63076923076923,-0.615384615384615,-0.6,-0.584615384615384,-0.569230769230769,
-0.553846153846154,-0.538461538461538,-0.523076923076923,-0.507692307692308,
-0.492307692307692,-0.476923076923077,-0.461538461538462,-0.446153846153846,
-0.430769230769231,-0.415384615384615,-0.4,-0.384615384615385,-0.369230769230769,
-0.353846153846154,-0.338461538461538,-0.323076923076923,-0.307692307692308,
-0.292307692307692,-0.276923076923077,-0.261538461538462,-0.246153846153846,
-0.230769230769231,-0.215384615384615,-0.2,-0.184615384615385,-0.169230769230769,
-0.153846153846154,-0.138461538461538,-0.123076923076923,-0.107692307692308,
-0.0923076923076923,-0.0769230769230769,-0.0615384615384615,-0.0461538461538462,
-0.0307692307692308,-0.0153846153846154,0.),(-1.,1.),.UNSPECIFIED.)
GEOMETRIC_REPRESENTATION_ITEM()
RATIONAL_B_SPLINE_SURFACE(((1.,1.),(1.,1.),(1.,1.),(1.,1.),(1.,1.),(1.,
1.),(1.,1.),(1.,1.),(1.,1.),(1.,1.),(1.,1.),(1.,1.),(1.,1.),(1.,1.),(1.,
1.),(1.,1.),(1.,1.),(1.,1.),(1.,1.),(1.,1.),(1.,1.),(1.,1.),(1.,1.),(1.,
1.),(1.,1.),(1.,1.),(1.,1.),(1.,1.),(1.,1.),(1.,1.),(1.,1.),(1.,1.),(1.,
1.),(1.,1.),(1.,1.),(1.,1.),(1.,1.),(1.,1.),(1.,1.),(1.,1.),(1.,1.),(1.,
1.),(1.,1.),(1.,1.),(1.,1.),(1.,1.),(1.,1.),(1.,1.),(1.,1.),(1.,1.),(1.,
1.),(1.,1.),(1.,1.),(1.,1.),(1.,1.),(1.,1.),(1.,1.),(1.,1.),(1.,1.),(1.,
1.),(1.,1.),(1.,1.),(1.,1.),(1.,1.),(1.,1.),(1.,1.),(1.,1.),(1.,1.),(1.,
1.),(1.,1.)))
REPRESENTATION_ITEM('')
SURFACE()
);
#17=(
BOUNDED_SURFACE()
B_SPLINE_SURFACE(5,1,((#25072,#25073),(#25074,#25075),(#25076,#25077),(#25078,
#25079),(#25080,#25081),(#25082,#25083),(#25084,#25085),(#25086,#25087),
(#25088,#25089),(#25090,#25091),(#25092,#25093),(#25094,#25095),(#25096,
#25097),(#25098,#25099),(#25100,#25101),(#25102,#25103),(#25104,#25105),
(#25106,#25107),(#25108,#25109),(#25110,#25111),(#25112,#25113),(#25114,
#25115),(#25116,#25117),(#25118,#25119),(#25120,#25121),(#25122,#25123),
(#25124,#25125),(#25126,#25127),(#25128,#25129),(#25130,#25131),(#25132,
#25133),(#25134,#25135),(#25136,#25137),(#25138,#25139),(#25140,#25141),
(#25142,#25143),(#25144,#25145),(#25146,#25147),(#25148,#25149),(#25150,
#25151),(#25152,#25153),(#25154,#25155),(#25156,#25157),(#25158,#25159),
(#25160,#25161),(#25162,#25163),(#25164,#25165),(#25166,#25167),(#25168,
#25169),(#25170,#25171),(#25172,#25173),(#25174,#25175),(#25176,#25177),
(#25178,#25179),(#25180,#25181),(#25182,#25183),(#25184,#25185),(#25186,
#25187),(#25188,#25189),(#25190,#25191),(#25192,#25193),(#25194,#25195),
(#25196,#25197),(#25198,#25199),(#25200,#25201),(#25202,#25203),(#25204,
#25205),(#25206,#25207),(#25208,#25209),(#25210,#25211)),.UNSPECIFIED.,
 .F.,.F.,.F.)
B_SPLINE_SURFACE_WITH_KNOTS((6,1,1,1,1,1,1,1,1,1,1,1,1,1,1,1,1,1,1,1,1,
1,1,1,1,1,1,1,1,1,1,1,1,1,1,1,1,1,1,1,1,1,1,1,1,1,1,1,1,1,1,1,1,1,1,1,1,
1,1,1,1,1,1,1,1,6),(2,2),(-1.,-0.984615384615383,-0.969230769230768,-0.953846153846152,
-0.938461538461537,-0.923076923076922,-0.907692307692306,-0.892307692307691,
-0.876923076923076,-0.86153846153846,-0.846153846153845,-0.83076923076923,
-0.815384615384614,-0.799999999999999,-0.784615384615384,-0.769230769230768,
-0.753846153846153,-0.738461538461538,-0.723076923076922,-0.707692307692307,
-0.692307692307692,-0.676923076923076,-0.661538461538461,-0.646153846153846,
-0.63076923076923,-0.615384615384615,-0.6,-0.584615384615384,-0.569230769230769,
-0.553846153846154,-0.538461538461538,-0.523076923076923,-0.507692307692308,
-0.492307692307692,-0.476923076923077,-0.461538461538462,-0.446153846153846,
-0.430769230769231,-0.415384615384615,-0.4,-0.384615384615385,-0.369230769230769,
-0.353846153846154,-0.338461538461538,-0.323076923076923,-0.307692307692308,
-0.292307692307692,-0.276923076923077,-0.261538461538462,-0.246153846153846,
-0.230769230769231,-0.215384615384615,-0.2,-0.184615384615385,-0.169230769230769,
-0.153846153846154,-0.138461538461538,-0.123076923076923,-0.107692307692308,
-0.0923076923076923,-0.0769230769230769,-0.0615384615384615,-0.0461538461538462,
-0.0307692307692308,-0.0153846153846154,0.),(-1.,1.),.UNSPECIFIED.)
GEOMETRIC_REPRESENTATION_ITEM()
RATIONAL_B_SPLINE_SURFACE(((1.,1.),(1.,1.),(1.,1.),(1.,1.),(1.,1.),(1.,
1.),(1.,1.),(1.,1.),(1.,1.),(1.,1.),(1.,1.),(1.,1.),(1.,1.),(1.,1.),(1.,
1.),(1.,1.),(1.,1.),(1.,1.),(1.,1.),(1.,1.),(1.,1.),(1.,1.),(1.,1.),(1.,
1.),(1.,1.),(1.,1.),(1.,1.),(1.,1.),(1.,1.),(1.,1.),(1.,1.),(1.,1.),(1.,
1.),(1.,1.),(1.,1.),(1.,1.),(1.,1.),(1.,1.),(1.,1.),(1.,1.),(1.,1.),(1.,
1.),(1.,1.),(1.,1.),(1.,1.),(1.,1.),(1.,1.),(1.,1.),(1.,1.),(1.,1.),(1.,
1.),(1.,1.),(1.,1.),(1.,1.),(1.,1.),(1.,1.),(1.,1.),(1.,1.),(1.,1.),(1.,
1.),(1.,1.),(1.,1.),(1.,1.),(1.,1.),(1.,1.),(1.,1.),(1.,1.),(1.,1.),(1.,
1.),(1.,1.)))
REPRESENTATION_ITEM('')
SURFACE()
);
#18=(
BOUNDED_SURFACE()
B_SPLINE_SURFACE(5,1,((#25288,#25289),(#25290,#25291),(#25292,#25293),(#25294,
#25295),(#25296,#25297),(#25298,#25299),(#25300,#25301),(#25302,#25303),
(#25304,#25305),(#25306,#25307),(#25308,#25309),(#25310,#25311),(#25312,
#25313),(#25314,#25315),(#25316,#25317),(#25318,#25319),(#25320,#25321),
(#25322,#25323),(#25324,#25325),(#25326,#25327),(#25328,#25329),(#25330,
#25331),(#25332,#25333),(#25334,#25335),(#25336,#25337),(#25338,#25339),
(#25340,#25341),(#25342,#25343),(#25344,#25345),(#25346,#25347),(#25348,
#25349),(#25350,#25351),(#25352,#25353),(#25354,#25355),(#25356,#25357),
(#25358,#25359),(#25360,#25361),(#25362,#25363),(#25364,#25365),(#25366,
#25367),(#25368,#25369),(#25370,#25371),(#25372,#25373),(#25374,#25375),
(#25376,#25377),(#25378,#25379),(#25380,#25381),(#25382,#25383),(#25384,
#25385),(#25386,#25387),(#25388,#25389),(#25390,#25391),(#25392,#25393),
(#25394,#25395),(#25396,#25397),(#25398,#25399),(#25400,#25401),(#25402,
#25403),(#25404,#25405),(#25406,#25407),(#25408,#25409),(#25410,#25411),
(#25412,#25413),(#25414,#25415),(#25416,#25417),(#25418,#25419),(#25420,
#25421),(#25422,#25423),(#25424,#25425),(#25426,#25427)),.UNSPECIFIED.,
 .F.,.F.,.F.)
B_SPLINE_SURFACE_WITH_KNOTS((6,1,1,1,1,1,1,1,1,1,1,1,1,1,1,1,1,1,1,1,1,
1,1,1,1,1,1,1,1,1,1,1,1,1,1,1,1,1,1,1,1,1,1,1,1,1,1,1,1,1,1,1,1,1,1,1,1,
1,1,1,1,1,1,1,1,6),(2,2),(-1.,-0.984615384615383,-0.969230769230768,-0.953846153846152,
-0.938461538461537,-0.923076923076922,-0.907692307692306,-0.892307692307691,
-0.876923076923076,-0.86153846153846,-0.846153846153845,-0.83076923076923,
-0.815384615384614,-0.799999999999999,-0.784615384615384,-0.769230769230768,
-0.753846153846153,-0.738461538461538,-0.723076923076922,-0.707692307692307,
-0.692307692307692,-0.676923076923076,-0.661538461538461,-0.646153846153846,
-0.63076923076923,-0.615384615384615,-0.6,-0.584615384615384,-0.569230769230769,
-0.553846153846154,-0.538461538461538,-0.523076923076923,-0.507692307692308,
-0.492307692307692,-0.476923076923077,-0.461538461538462,-0.446153846153846,
-0.430769230769231,-0.415384615384615,-0.4,-0.384615384615385,-0.369230769230769,
-0.353846153846154,-0.338461538461538,-0.323076923076923,-0.307692307692308,
-0.292307692307692,-0.276923076923077,-0.261538461538462,-0.246153846153846,
-0.230769230769231,-0.215384615384615,-0.2,-0.184615384615385,-0.169230769230769,
-0.153846153846154,-0.138461538461538,-0.123076923076923,-0.107692307692308,
-0.0923076923076923,-0.0769230769230769,-0.0615384615384615,-0.0461538461538462,
-0.0307692307692308,-0.0153846153846154,0.),(-1.,1.),.UNSPECIFIED.)
GEOMETRIC_REPRESENTATION_ITEM()
RATIONAL_B_SPLINE_SURFACE(((1.,1.),(1.,1.),(1.,1.),(1.,1.),(1.,1.),(1.,
1.),(1.,1.),(1.,1.),(1.,1.),(1.,1.),(1.,1.),(1.,1.),(1.,1.),(1.,1.),(1.,
1.),(1.,1.),(1.,1.),(1.,1.),(1.,1.),(1.,1.),(1.,1.),(1.,1.),(1.,1.),(1.,
1.),(1.,1.),(1.,1.),(1.,1.),(1.,1.),(1.,1.),(1.,1.),(1.,1.),(1.,1.),(1.,
1.),(1.,1.),(1.,1.),(1.,1.),(1.,1.),(1.,1.),(1.,1.),(1.,1.),(1.,1.),(1.,
1.),(1.,1.),(1.,1.),(1.,1.),(1.,1.),(1.,1.),(1.,1.),(1.,1.),(1.,1.),(1.,
1.),(1.,1.),(1.,1.),(1.,1.),(1.,1.),(1.,1.),(1.,1.),(1.,1.),(1.,1.),(1.,
1.),(1.,1.),(1.,1.),(1.,1.),(1.,1.),(1.,1.),(1.,1.),(1.,1.),(1.,1.),(1.,
1.),(1.,1.)))
REPRESENTATION_ITEM('')
SURFACE()
);
#19=(
BOUNDED_SURFACE()
B_SPLINE_SURFACE(5,1,((#25504,#25505),(#25506,#25507),(#25508,#25509),(#25510,
#25511),(#25512,#25513),(#25514,#25515),(#25516,#25517),(#25518,#25519),
(#25520,#25521),(#25522,#25523),(#25524,#25525),(#25526,#25527),(#25528,
#25529),(#25530,#25531),(#25532,#25533),(#25534,#25535),(#25536,#25537),
(#25538,#25539),(#25540,#25541),(#25542,#25543),(#25544,#25545),(#25546,
#25547),(#25548,#25549),(#25550,#25551),(#25552,#25553),(#25554,#25555),
(#25556,#25557),(#25558,#25559),(#25560,#25561),(#25562,#25563),(#25564,
#25565),(#25566,#25567),(#25568,#25569),(#25570,#25571),(#25572,#25573),
(#25574,#25575),(#25576,#25577),(#25578,#25579),(#25580,#25581),(#25582,
#25583),(#25584,#25585),(#25586,#25587),(#25588,#25589),(#25590,#25591),
(#25592,#25593),(#25594,#25595),(#25596,#25597),(#25598,#25599),(#25600,
#25601),(#25602,#25603),(#25604,#25605),(#25606,#25607),(#25608,#25609),
(#25610,#25611),(#25612,#25613),(#25614,#25615),(#25616,#25617),(#25618,
#25619),(#25620,#25621),(#25622,#25623),(#25624,#25625),(#25626,#25627),
(#25628,#25629),(#25630,#25631),(#25632,#25633),(#25634,#25635),(#25636,
#25637),(#25638,#25639),(#25640,#25641),(#25642,#25643)),.UNSPECIFIED.,
 .F.,.F.,.F.)
B_SPLINE_SURFACE_WITH_KNOTS((6,1,1,1,1,1,1,1,1,1,1,1,1,1,1,1,1,1,1,1,1,
1,1,1,1,1,1,1,1,1,1,1,1,1,1,1,1,1,1,1,1,1,1,1,1,1,1,1,1,1,1,1,1,1,1,1,1,
1,1,1,1,1,1,1,1,6),(2,2),(-1.,-0.984615384615383,-0.969230769230768,-0.953846153846152,
-0.938461538461537,-0.923076923076922,-0.907692307692306,-0.892307692307691,
-0.876923076923076,-0.86153846153846,-0.846153846153845,-0.83076923076923,
-0.815384615384614,-0.799999999999999,-0.784615384615384,-0.769230769230768,
-0.753846153846153,-0.738461538461538,-0.723076923076922,-0.707692307692307,
-0.692307692307692,-0.676923076923076,-0.661538461538461,-0.646153846153846,
-0.63076923076923,-0.615384615384615,-0.6,-0.584615384615384,-0.569230769230769,
-0.553846153846154,-0.538461538461538,-0.523076923076923,-0.507692307692308,
-0.492307692307692,-0.476923076923077,-0.461538461538462,-0.446153846153846,
-0.430769230769231,-0.415384615384615,-0.4,-0.384615384615385,-0.369230769230769,
-0.353846153846154,-0.338461538461538,-0.323076923076923,-0.307692307692308,
-0.292307692307692,-0.276923076923077,-0.261538461538462,-0.246153846153846,
-0.230769230769231,-0.215384615384615,-0.2,-0.184615384615385,-0.169230769230769,
-0.153846153846154,-0.138461538461538,-0.123076923076923,-0.107692307692308,
-0.0923076923076923,-0.0769230769230769,-0.0615384615384615,-0.0461538461538462,
-0.0307692307692308,-0.0153846153846154,0.),(-1.,1.),.UNSPECIFIED.)
GEOMETRIC_REPRESENTATION_ITEM()
RATIONAL_B_SPLINE_SURFACE(((1.,1.),(1.,1.),(1.,1.),(1.,1.),(1.,1.),(1.,
1.),(1.,1.),(1.,1.),(1.,1.),(1.,1.),(1.,1.),(1.,1.),(1.,1.),(1.,1.),(1.,
1.),(1.,1.),(1.,1.),(1.,1.),(1.,1.),(1.,1.),(1.,1.),(1.,1.),(1.,1.),(1.,
1.),(1.,1.),(1.,1.),(1.,1.),(1.,1.),(1.,1.),(1.,1.),(1.,1.),(1.,1.),(1.,
1.),(1.,1.),(1.,1.),(1.,1.),(1.,1.),(1.,1.),(1.,1.),(1.,1.),(1.,1.),(1.,
1.),(1.,1.),(1.,1.),(1.,1.),(1.,1.),(1.,1.),(1.,1.),(1.,1.),(1.,1.),(1.,
1.),(1.,1.),(1.,1.),(1.,1.),(1.,1.),(1.,1.),(1.,1.),(1.,1.),(1.,1.),(1.,
1.),(1.,1.),(1.,1.),(1.,1.),(1.,1.),(1.,1.),(1.,1.),(1.,1.),(1.,1.),(1.,
1.),(1.,1.)))
REPRESENTATION_ITEM('')
SURFACE()
);
#20=(
BOUNDED_SURFACE()
B_SPLINE_SURFACE(5,1,((#25720,#25721),(#25722,#25723),(#25724,#25725),(#25726,
#25727),(#25728,#25729),(#25730,#25731),(#25732,#25733),(#25734,#25735),
(#25736,#25737),(#25738,#25739),(#25740,#25741),(#25742,#25743),(#25744,
#25745),(#25746,#25747),(#25748,#25749),(#25750,#25751),(#25752,#25753),
(#25754,#25755),(#25756,#25757),(#25758,#25759),(#25760,#25761),(#25762,
#25763),(#25764,#25765),(#25766,#25767),(#25768,#25769),(#25770,#25771),
(#25772,#25773),(#25774,#25775),(#25776,#25777),(#25778,#25779),(#25780,
#25781),(#25782,#25783),(#25784,#25785),(#25786,#25787),(#25788,#25789),
(#25790,#25791),(#25792,#25793),(#25794,#25795),(#25796,#25797),(#25798,
#25799),(#25800,#25801),(#25802,#25803),(#25804,#25805),(#25806,#25807),
(#25808,#25809),(#25810,#25811),(#25812,#25813),(#25814,#25815),(#25816,
#25817),(#25818,#25819),(#25820,#25821),(#25822,#25823),(#25824,#25825),
(#25826,#25827),(#25828,#25829),(#25830,#25831),(#25832,#25833),(#25834,
#25835),(#25836,#25837),(#25838,#25839),(#25840,#25841),(#25842,#25843),
(#25844,#25845),(#25846,#25847),(#25848,#25849),(#25850,#25851),(#25852,
#25853),(#25854,#25855),(#25856,#25857),(#25858,#25859)),.UNSPECIFIED.,
 .F.,.F.,.F.)
B_SPLINE_SURFACE_WITH_KNOTS((6,1,1,1,1,1,1,1,1,1,1,1,1,1,1,1,1,1,1,1,1,
1,1,1,1,1,1,1,1,1,1,1,1,1,1,1,1,1,1,1,1,1,1,1,1,1,1,1,1,1,1,1,1,1,1,1,1,
1,1,1,1,1,1,1,1,6),(2,2),(-1.,-0.984615384615383,-0.969230769230768,-0.953846153846152,
-0.938461538461537,-0.923076923076922,-0.907692307692306,-0.892307692307691,
-0.876923076923076,-0.86153846153846,-0.846153846153845,-0.83076923076923,
-0.815384615384614,-0.799999999999999,-0.784615384615384,-0.769230769230768,
-0.753846153846153,-0.738461538461538,-0.723076923076922,-0.707692307692307,
-0.692307692307692,-0.676923076923076,-0.661538461538461,-0.646153846153846,
-0.63076923076923,-0.615384615384615,-0.6,-0.584615384615384,-0.569230769230769,
-0.553846153846154,-0.538461538461538,-0.523076923076923,-0.507692307692308,
-0.492307692307692,-0.476923076923077,-0.461538461538462,-0.446153846153846,
-0.430769230769231,-0.415384615384615,-0.4,-0.384615384615385,-0.369230769230769,
-0.353846153846154,-0.338461538461538,-0.323076923076923,-0.307692307692308,
-0.292307692307692,-0.276923076923077,-0.261538461538462,-0.246153846153846,
-0.230769230769231,-0.215384615384615,-0.2,-0.184615384615385,-0.169230769230769,
-0.153846153846154,-0.138461538461538,-0.123076923076923,-0.107692307692308,
-0.0923076923076923,-0.0769230769230769,-0.0615384615384615,-0.0461538461538462,
-0.0307692307692308,-0.0153846153846154,0.),(-1.,1.),.UNSPECIFIED.)
GEOMETRIC_REPRESENTATION_ITEM()
RATIONAL_B_SPLINE_SURFACE(((1.,1.),(1.,1.),(1.,1.),(1.,1.),(1.,1.),(1.,
1.),(1.,1.),(1.,1.),(1.,1.),(1.,1.),(1.,1.),(1.,1.),(1.,1.),(1.,1.),(1.,
1.),(1.,1.),(1.,1.),(1.,1.),(1.,1.),(1.,1.),(1.,1.),(1.,1.),(1.,1.),(1.,
1.),(1.,1.),(1.,1.),(1.,1.),(1.,1.),(1.,1.),(1.,1.),(1.,1.),(1.,1.),(1.,
1.),(1.,1.),(1.,1.),(1.,1.),(1.,1.),(1.,1.),(1.,1.),(1.,1.),(1.,1.),(1.,
1.),(1.,1.),(1.,1.),(1.,1.),(1.,1.),(1.,1.),(1.,1.),(1.,1.),(1.,1.),(1.,
1.),(1.,1.),(1.,1.),(1.,1.),(1.,1.),(1.,1.),(1.,1.),(1.,1.),(1.,1.),(1.,
1.),(1.,1.),(1.,1.),(1.,1.),(1.,1.),(1.,1.),(1.,1.),(1.,1.),(1.,1.),(1.,
1.),(1.,1.)))
REPRESENTATION_ITEM('')
SURFACE()
);
#21=(
BOUNDED_SURFACE()
B_SPLINE_SURFACE(5,1,((#25936,#25937),(#25938,#25939),(#25940,#25941),(#25942,
#25943),(#25944,#25945),(#25946,#25947),(#25948,#25949),(#25950,#25951),
(#25952,#25953),(#25954,#25955),(#25956,#25957),(#25958,#25959),(#25960,
#25961),(#25962,#25963),(#25964,#25965),(#25966,#25967),(#25968,#25969),
(#25970,#25971),(#25972,#25973),(#25974,#25975),(#25976,#25977),(#25978,
#25979),(#25980,#25981),(#25982,#25983),(#25984,#25985),(#25986,#25987),
(#25988,#25989),(#25990,#25991),(#25992,#25993),(#25994,#25995),(#25996,
#25997),(#25998,#25999),(#26000,#26001),(#26002,#26003),(#26004,#26005),
(#26006,#26007),(#26008,#26009),(#26010,#26011),(#26012,#26013),(#26014,
#26015),(#26016,#26017),(#26018,#26019),(#26020,#26021),(#26022,#26023),
(#26024,#26025),(#26026,#26027),(#26028,#26029),(#26030,#26031),(#26032,
#26033),(#26034,#26035),(#26036,#26037),(#26038,#26039),(#26040,#26041),
(#26042,#26043),(#26044,#26045),(#26046,#26047),(#26048,#26049),(#26050,
#26051),(#26052,#26053),(#26054,#26055),(#26056,#26057),(#26058,#26059),
(#26060,#26061),(#26062,#26063),(#26064,#26065),(#26066,#26067),(#26068,
#26069),(#26070,#26071),(#26072,#26073),(#26074,#26075)),.UNSPECIFIED.,
 .F.,.F.,.F.)
B_SPLINE_SURFACE_WITH_KNOTS((6,1,1,1,1,1,1,1,1,1,1,1,1,1,1,1,1,1,1,1,1,
1,1,1,1,1,1,1,1,1,1,1,1,1,1,1,1,1,1,1,1,1,1,1,1,1,1,1,1,1,1,1,1,1,1,1,1,
1,1,1,1,1,1,1,1,6),(2,2),(-1.,-0.984615384615383,-0.969230769230768,-0.953846153846152,
-0.938461538461537,-0.923076923076922,-0.907692307692306,-0.892307692307691,
-0.876923076923076,-0.86153846153846,-0.846153846153845,-0.83076923076923,
-0.815384615384614,-0.799999999999999,-0.784615384615384,-0.769230769230768,
-0.753846153846153,-0.738461538461538,-0.723076923076922,-0.707692307692307,
-0.692307692307692,-0.676923076923076,-0.661538461538461,-0.646153846153846,
-0.63076923076923,-0.615384615384615,-0.6,-0.584615384615384,-0.569230769230769,
-0.553846153846154,-0.538461538461538,-0.523076923076923,-0.507692307692308,
-0.492307692307692,-0.476923076923077,-0.461538461538462,-0.446153846153846,
-0.430769230769231,-0.415384615384615,-0.4,-0.384615384615385,-0.369230769230769,
-0.353846153846154,-0.338461538461538,-0.323076923076923,-0.307692307692308,
-0.292307692307692,-0.276923076923077,-0.261538461538462,-0.246153846153846,
-0.230769230769231,-0.215384615384615,-0.2,-0.184615384615385,-0.169230769230769,
-0.153846153846154,-0.138461538461538,-0.123076923076923,-0.107692307692308,
-0.0923076923076923,-0.0769230769230769,-0.0615384615384615,-0.0461538461538462,
-0.0307692307692308,-0.0153846153846154,0.),(-1.,1.),.UNSPECIFIED.)
GEOMETRIC_REPRESENTATION_ITEM()
RATIONAL_B_SPLINE_SURFACE(((1.,1.),(1.,1.),(1.,1.),(1.,1.),(1.,1.),(1.,
1.),(1.,1.),(1.,1.),(1.,1.),(1.,1.),(1.,1.),(1.,1.),(1.,1.),(1.,1.),(1.,
1.),(1.,1.),(1.,1.),(1.,1.),(1.,1.),(1.,1.),(1.,1.),(1.,1.),(1.,1.),(1.,
1.),(1.,1.),(1.,1.),(1.,1.),(1.,1.),(1.,1.),(1.,1.),(1.,1.),(1.,1.),(1.,
1.),(1.,1.),(1.,1.),(1.,1.),(1.,1.),(1.,1.),(1.,1.),(1.,1.),(1.,1.),(1.,
1.),(1.,1.),(1.,1.),(1.,1.),(1.,1.),(1.,1.),(1.,1.),(1.,1.),(1.,1.),(1.,
1.),(1.,1.),(1.,1.),(1.,1.),(1.,1.),(1.,1.),(1.,1.),(1.,1.),(1.,1.),(1.,
1.),(1.,1.),(1.,1.),(1.,1.),(1.,1.),(1.,1.),(1.,1.),(1.,1.),(1.,1.),(1.,
1.),(1.,1.)))
REPRESENTATION_ITEM('')
SURFACE()
);
#22=(
BOUNDED_SURFACE()
B_SPLINE_SURFACE(5,1,((#26152,#26153),(#26154,#26155),(#26156,#26157),(#26158,
#26159),(#26160,#26161),(#26162,#26163),(#26164,#26165),(#26166,#26167),
(#26168,#26169),(#26170,#26171),(#26172,#26173),(#26174,#26175),(#26176,
#26177),(#26178,#26179),(#26180,#26181),(#26182,#26183),(#26184,#26185),
(#26186,#26187),(#26188,#26189),(#26190,#26191),(#26192,#26193),(#26194,
#26195),(#26196,#26197),(#26198,#26199),(#26200,#26201),(#26202,#26203),
(#26204,#26205),(#26206,#26207),(#26208,#26209),(#26210,#26211),(#26212,
#26213),(#26214,#26215),(#26216,#26217),(#26218,#26219),(#26220,#26221),
(#26222,#26223),(#26224,#26225),(#26226,#26227),(#26228,#26229),(#26230,
#26231),(#26232,#26233),(#26234,#26235),(#26236,#26237),(#26238,#26239),
(#26240,#26241),(#26242,#26243),(#26244,#26245),(#26246,#26247),(#26248,
#26249),(#26250,#26251),(#26252,#26253),(#26254,#26255),(#26256,#26257),
(#26258,#26259),(#26260,#26261),(#26262,#26263),(#26264,#26265),(#26266,
#26267),(#26268,#26269),(#26270,#26271),(#26272,#26273),(#26274,#26275),
(#26276,#26277),(#26278,#26279),(#26280,#26281),(#26282,#26283),(#26284,
#26285),(#26286,#26287),(#26288,#26289),(#26290,#26291)),.UNSPECIFIED.,
 .F.,.F.,.F.)
B_SPLINE_SURFACE_WITH_KNOTS((6,1,1,1,1,1,1,1,1,1,1,1,1,1,1,1,1,1,1,1,1,
1,1,1,1,1,1,1,1,1,1,1,1,1,1,1,1,1,1,1,1,1,1,1,1,1,1,1,1,1,1,1,1,1,1,1,1,
1,1,1,1,1,1,1,1,6),(2,2),(-1.,-0.984615384615383,-0.969230769230768,-0.953846153846152,
-0.938461538461537,-0.923076923076922,-0.907692307692306,-0.892307692307691,
-0.876923076923076,-0.86153846153846,-0.846153846153845,-0.83076923076923,
-0.815384615384614,-0.799999999999999,-0.784615384615384,-0.769230769230768,
-0.753846153846153,-0.738461538461538,-0.723076923076922,-0.707692307692307,
-0.692307692307692,-0.676923076923076,-0.661538461538461,-0.646153846153846,
-0.63076923076923,-0.615384615384615,-0.6,-0.584615384615384,-0.569230769230769,
-0.553846153846154,-0.538461538461538,-0.523076923076923,-0.507692307692308,
-0.492307692307692,-0.476923076923077,-0.461538461538462,-0.446153846153846,
-0.430769230769231,-0.415384615384615,-0.4,-0.384615384615385,-0.369230769230769,
-0.353846153846154,-0.338461538461538,-0.323076923076923,-0.307692307692308,
-0.292307692307692,-0.276923076923077,-0.261538461538462,-0.246153846153846,
-0.230769230769231,-0.215384615384615,-0.2,-0.184615384615385,-0.169230769230769,
-0.153846153846154,-0.138461538461538,-0.123076923076923,-0.107692307692308,
-0.0923076923076923,-0.0769230769230769,-0.0615384615384615,-0.0461538461538462,
-0.0307692307692308,-0.0153846153846154,0.),(-1.,1.),.UNSPECIFIED.)
GEOMETRIC_REPRESENTATION_ITEM()
RATIONAL_B_SPLINE_SURFACE(((1.,1.),(1.,1.),(1.,1.),(1.,1.),(1.,1.),(1.,
1.),(1.,1.),(1.,1.),(1.,1.),(1.,1.),(1.,1.),(1.,1.),(1.,1.),(1.,1.),(1.,
1.),(1.,1.),(1.,1.),(1.,1.),(1.,1.),(1.,1.),(1.,1.),(1.,1.),(1.,1.),(1.,
1.),(1.,1.),(1.,1.),(1.,1.),(1.,1.),(1.,1.),(1.,1.),(1.,1.),(1.,1.),(1.,
1.),(1.,1.),(1.,1.),(1.,1.),(1.,1.),(1.,1.),(1.,1.),(1.,1.),(1.,1.),(1.,
1.),(1.,1.),(1.,1.),(1.,1.),(1.,1.),(1.,1.),(1.,1.),(1.,1.),(1.,1.),(1.,
1.),(1.,1.),(1.,1.),(1.,1.),(1.,1.),(1.,1.),(1.,1.),(1.,1.),(1.,1.),(1.,
1.),(1.,1.),(1.,1.),(1.,1.),(1.,1.),(1.,1.),(1.,1.),(1.,1.),(1.,1.),(1.,
1.),(1.,1.)))
REPRESENTATION_ITEM('')
SURFACE()
);
#23=(
BOUNDED_SURFACE()
B_SPLINE_SURFACE(5,1,((#26368,#26369),(#26370,#26371),(#26372,#26373),(#26374,
#26375),(#26376,#26377),(#26378,#26379),(#26380,#26381),(#26382,#26383),
(#26384,#26385),(#26386,#26387),(#26388,#26389),(#26390,#26391),(#26392,
#26393),(#26394,#26395),(#26396,#26397),(#26398,#26399),(#26400,#26401),
(#26402,#26403),(#26404,#26405),(#26406,#26407),(#26408,#26409),(#26410,
#26411),(#26412,#26413),(#26414,#26415),(#26416,#26417),(#26418,#26419),
(#26420,#26421),(#26422,#26423),(#26424,#26425),(#26426,#26427),(#26428,
#26429),(#26430,#26431),(#26432,#26433),(#26434,#26435),(#26436,#26437),
(#26438,#26439),(#26440,#26441),(#26442,#26443),(#26444,#26445),(#26446,
#26447),(#26448,#26449),(#26450,#26451),(#26452,#26453),(#26454,#26455),
(#26456,#26457),(#26458,#26459),(#26460,#26461),(#26462,#26463),(#26464,
#26465),(#26466,#26467),(#26468,#26469),(#26470,#26471),(#26472,#26473),
(#26474,#26475),(#26476,#26477),(#26478,#26479),(#26480,#26481),(#26482,
#26483),(#26484,#26485),(#26486,#26487),(#26488,#26489),(#26490,#26491),
(#26492,#26493),(#26494,#26495),(#26496,#26497),(#26498,#26499),(#26500,
#26501),(#26502,#26503),(#26504,#26505),(#26506,#26507)),.UNSPECIFIED.,
 .F.,.F.,.F.)
B_SPLINE_SURFACE_WITH_KNOTS((6,1,1,1,1,1,1,1,1,1,1,1,1,1,1,1,1,1,1,1,1,
1,1,1,1,1,1,1,1,1,1,1,1,1,1,1,1,1,1,1,1,1,1,1,1,1,1,1,1,1,1,1,1,1,1,1,1,
1,1,1,1,1,1,1,1,6),(2,2),(-1.,-0.984615384615383,-0.969230769230768,-0.953846153846152,
-0.938461538461537,-0.923076923076922,-0.907692307692306,-0.892307692307691,
-0.876923076923076,-0.86153846153846,-0.846153846153845,-0.83076923076923,
-0.815384615384614,-0.799999999999999,-0.784615384615384,-0.769230769230768,
-0.753846153846153,-0.738461538461538,-0.723076923076922,-0.707692307692307,
-0.692307692307692,-0.676923076923076,-0.661538461538461,-0.646153846153846,
-0.63076923076923,-0.615384615384615,-0.6,-0.584615384615384,-0.569230769230769,
-0.553846153846154,-0.538461538461538,-0.523076923076923,-0.507692307692308,
-0.492307692307692,-0.476923076923077,-0.461538461538462,-0.446153846153846,
-0.430769230769231,-0.415384615384615,-0.4,-0.384615384615385,-0.369230769230769,
-0.353846153846154,-0.338461538461538,-0.323076923076923,-0.307692307692308,
-0.292307692307692,-0.276923076923077,-0.261538461538462,-0.246153846153846,
-0.230769230769231,-0.215384615384615,-0.2,-0.184615384615385,-0.169230769230769,
-0.153846153846154,-0.138461538461538,-0.123076923076923,-0.107692307692308,
-0.0923076923076923,-0.0769230769230769,-0.0615384615384615,-0.0461538461538462,
-0.0307692307692308,-0.0153846153846154,0.),(-1.,1.),.UNSPECIFIED.)
GEOMETRIC_REPRESENTATION_ITEM()
RATIONAL_B_SPLINE_SURFACE(((1.,1.),(1.,1.),(1.,1.),(1.,1.),(1.,1.),(1.,
1.),(1.,1.),(1.,1.),(1.,1.),(1.,1.),(1.,1.),(1.,1.),(1.,1.),(1.,1.),(1.,
1.),(1.,1.),(1.,1.),(1.,1.),(1.,1.),(1.,1.),(1.,1.),(1.,1.),(1.,1.),(1.,
1.),(1.,1.),(1.,1.),(1.,1.),(1.,1.),(1.,1.),(1.,1.),(1.,1.),(1.,1.),(1.,
1.),(1.,1.),(1.,1.),(1.,1.),(1.,1.),(1.,1.),(1.,1.),(1.,1.),(1.,1.),(1.,
1.),(1.,1.),(1.,1.),(1.,1.),(1.,1.),(1.,1.),(1.,1.),(1.,1.),(1.,1.),(1.,
1.),(1.,1.),(1.,1.),(1.,1.),(1.,1.),(1.,1.),(1.,1.),(1.,1.),(1.,1.),(1.,
1.),(1.,1.),(1.,1.),(1.,1.),(1.,1.),(1.,1.),(1.,1.),(1.,1.),(1.,1.),(1.,
1.),(1.,1.)))
REPRESENTATION_ITEM('')
SURFACE()
);
#24=(
BOUNDED_SURFACE()
B_SPLINE_SURFACE(5,1,((#26584,#26585),(#26586,#26587),(#26588,#26589),(#26590,
#26591),(#26592,#26593),(#26594,#26595),(#26596,#26597),(#26598,#26599),
(#26600,#26601),(#26602,#26603),(#26604,#26605),(#26606,#26607),(#26608,
#26609),(#26610,#26611),(#26612,#26613),(#26614,#26615),(#26616,#26617),
(#26618,#26619),(#26620,#26621),(#26622,#26623),(#26624,#26625),(#26626,
#26627),(#26628,#26629),(#26630,#26631),(#26632,#26633),(#26634,#26635),
(#26636,#26637),(#26638,#26639),(#26640,#26641),(#26642,#26643),(#26644,
#26645),(#26646,#26647),(#26648,#26649),(#26650,#26651),(#26652,#26653),
(#26654,#26655),(#26656,#26657),(#26658,#26659),(#26660,#26661),(#26662,
#26663),(#26664,#26665),(#26666,#26667),(#26668,#26669),(#26670,#26671),
(#26672,#26673),(#26674,#26675),(#26676,#26677),(#26678,#26679),(#26680,
#26681),(#26682,#26683),(#26684,#26685),(#26686,#26687),(#26688,#26689),
(#26690,#26691),(#26692,#26693),(#26694,#26695),(#26696,#26697),(#26698,
#26699),(#26700,#26701),(#26702,#26703),(#26704,#26705),(#26706,#26707),
(#26708,#26709),(#26710,#26711),(#26712,#26713),(#26714,#26715),(#26716,
#26717),(#26718,#26719),(#26720,#26721),(#26722,#26723)),.UNSPECIFIED.,
 .F.,.F.,.F.)
B_SPLINE_SURFACE_WITH_KNOTS((6,1,1,1,1,1,1,1,1,1,1,1,1,1,1,1,1,1,1,1,1,
1,1,1,1,1,1,1,1,1,1,1,1,1,1,1,1,1,1,1,1,1,1,1,1,1,1,1,1,1,1,1,1,1,1,1,1,
1,1,1,1,1,1,1,1,6),(2,2),(-1.,-0.984615384615383,-0.969230769230768,-0.953846153846152,
-0.938461538461537,-0.923076923076922,-0.907692307692306,-0.892307692307691,
-0.876923076923076,-0.86153846153846,-0.846153846153845,-0.83076923076923,
-0.815384615384614,-0.799999999999999,-0.784615384615384,-0.769230769230768,
-0.753846153846153,-0.738461538461538,-0.723076923076922,-0.707692307692307,
-0.692307692307692,-0.676923076923076,-0.661538461538461,-0.646153846153846,
-0.63076923076923,-0.615384615384615,-0.6,-0.584615384615384,-0.569230769230769,
-0.553846153846154,-0.538461538461538,-0.523076923076923,-0.507692307692308,
-0.492307692307692,-0.476923076923077,-0.461538461538462,-0.446153846153846,
-0.430769230769231,-0.415384615384615,-0.4,-0.384615384615385,-0.369230769230769,
-0.353846153846154,-0.338461538461538,-0.323076923076923,-0.307692307692308,
-0.292307692307692,-0.276923076923077,-0.261538461538462,-0.246153846153846,
-0.230769230769231,-0.215384615384615,-0.2,-0.184615384615385,-0.169230769230769,
-0.153846153846154,-0.138461538461538,-0.123076923076923,-0.107692307692308,
-0.0923076923076923,-0.0769230769230769,-0.0615384615384615,-0.0461538461538462,
-0.0307692307692308,-0.0153846153846154,0.),(-1.,1.),.UNSPECIFIED.)
GEOMETRIC_REPRESENTATION_ITEM()
RATIONAL_B_SPLINE_SURFACE(((1.,1.),(1.,1.),(1.,1.),(1.,1.),(1.,1.),(1.,
1.),(1.,1.),(1.,1.),(1.,1.),(1.,1.),(1.,1.),(1.,1.),(1.,1.),(1.,1.),(1.,
1.),(1.,1.),(1.,1.),(1.,1.),(1.,1.),(1.,1.),(1.,1.),(1.,1.),(1.,1.),(1.,
1.),(1.,1.),(1.,1.),(1.,1.),(1.,1.),(1.,1.),(1.,1.),(1.,1.),(1.,1.),(1.,
1.),(1.,1.),(1.,1.),(1.,1.),(1.,1.),(1.,1.),(1.,1.),(1.,1.),(1.,1.),(1.,
1.),(1.,1.),(1.,1.),(1.,1.),(1.,1.),(1.,1.),(1.,1.),(1.,1.),(1.,1.),(1.,
1.),(1.,1.),(1.,1.),(1.,1.),(1.,1.),(1.,1.),(1.,1.),(1.,1.),(1.,1.),(1.,
1.),(1.,1.),(1.,1.),(1.,1.),(1.,1.),(1.,1.),(1.,1.),(1.,1.),(1.,1.),(1.,
1.),(1.,1.)))
REPRESENTATION_ITEM('')
SURFACE()
);
#25=(
BOUNDED_SURFACE()
B_SPLINE_SURFACE(5,1,((#26800,#26801),(#26802,#26803),(#26804,#26805),(#26806,
#26807),(#26808,#26809),(#26810,#26811),(#26812,#26813),(#26814,#26815),
(#26816,#26817),(#26818,#26819),(#26820,#26821),(#26822,#26823),(#26824,
#26825),(#26826,#26827),(#26828,#26829),(#26830,#26831),(#26832,#26833),
(#26834,#26835),(#26836,#26837),(#26838,#26839),(#26840,#26841),(#26842,
#26843),(#26844,#26845),(#26846,#26847),(#26848,#26849),(#26850,#26851),
(#26852,#26853),(#26854,#26855),(#26856,#26857),(#26858,#26859),(#26860,
#26861),(#26862,#26863),(#26864,#26865),(#26866,#26867),(#26868,#26869),
(#26870,#26871),(#26872,#26873),(#26874,#26875),(#26876,#26877),(#26878,
#26879),(#26880,#26881),(#26882,#26883),(#26884,#26885),(#26886,#26887),
(#26888,#26889),(#26890,#26891),(#26892,#26893),(#26894,#26895),(#26896,
#26897),(#26898,#26899),(#26900,#26901),(#26902,#26903),(#26904,#26905),
(#26906,#26907),(#26908,#26909),(#26910,#26911),(#26912,#26913),(#26914,
#26915),(#26916,#26917),(#26918,#26919),(#26920,#26921),(#26922,#26923),
(#26924,#26925),(#26926,#26927),(#26928,#26929),(#26930,#26931),(#26932,
#26933),(#26934,#26935),(#26936,#26937),(#26938,#26939)),.UNSPECIFIED.,
 .F.,.F.,.F.)
B_SPLINE_SURFACE_WITH_KNOTS((6,1,1,1,1,1,1,1,1,1,1,1,1,1,1,1,1,1,1,1,1,
1,1,1,1,1,1,1,1,1,1,1,1,1,1,1,1,1,1,1,1,1,1,1,1,1,1,1,1,1,1,1,1,1,1,1,1,
1,1,1,1,1,1,1,1,6),(2,2),(-1.,-0.984615384615383,-0.969230769230768,-0.953846153846152,
-0.938461538461537,-0.923076923076922,-0.907692307692306,-0.892307692307691,
-0.876923076923076,-0.86153846153846,-0.846153846153845,-0.83076923076923,
-0.815384615384614,-0.799999999999999,-0.784615384615384,-0.769230769230768,
-0.753846153846153,-0.738461538461538,-0.723076923076922,-0.707692307692307,
-0.692307692307692,-0.676923076923076,-0.661538461538461,-0.646153846153846,
-0.63076923076923,-0.615384615384615,-0.6,-0.584615384615384,-0.569230769230769,
-0.553846153846154,-0.538461538461538,-0.523076923076923,-0.507692307692308,
-0.492307692307692,-0.476923076923077,-0.461538461538462,-0.446153846153846,
-0.430769230769231,-0.415384615384615,-0.4,-0.384615384615385,-0.369230769230769,
-0.353846153846154,-0.338461538461538,-0.323076923076923,-0.307692307692308,
-0.292307692307692,-0.276923076923077,-0.261538461538462,-0.246153846153846,
-0.230769230769231,-0.215384615384615,-0.2,-0.184615384615385,-0.169230769230769,
-0.153846153846154,-0.138461538461538,-0.123076923076923,-0.107692307692308,
-0.0923076923076923,-0.0769230769230769,-0.0615384615384615,-0.0461538461538462,
-0.0307692307692308,-0.0153846153846154,0.),(-1.,1.),.UNSPECIFIED.)
GEOMETRIC_REPRESENTATION_ITEM()
RATIONAL_B_SPLINE_SURFACE(((1.,1.),(1.,1.),(1.,1.),(1.,1.),(1.,1.),(1.,
1.),(1.,1.),(1.,1.),(1.,1.),(1.,1.),(1.,1.),(1.,1.),(1.,1.),(1.,1.),(1.,
1.),(1.,1.),(1.,1.),(1.,1.),(1.,1.),(1.,1.),(1.,1.),(1.,1.),(1.,1.),(1.,
1.),(1.,1.),(1.,1.),(1.,1.),(1.,1.),(1.,1.),(1.,1.),(1.,1.),(1.,1.),(1.,
1.),(1.,1.),(1.,1.),(1.,1.),(1.,1.),(1.,1.),(1.,1.),(1.,1.),(1.,1.),(1.,
1.),(1.,1.),(1.,1.),(1.,1.),(1.,1.),(1.,1.),(1.,1.),(1.,1.),(1.,1.),(1.,
1.),(1.,1.),(1.,1.),(1.,1.),(1.,1.),(1.,1.),(1.,1.),(1.,1.),(1.,1.),(1.,
1.),(1.,1.),(1.,1.),(1.,1.),(1.,1.),(1.,1.),(1.,1.),(1.,1.),(1.,1.),(1.,
1.),(1.,1.)))
REPRESENTATION_ITEM('')
SURFACE()
);
#26=(
BOUNDED_SURFACE()
B_SPLINE_SURFACE(5,1,((#27016,#27017),(#27018,#27019),(#27020,#27021),(#27022,
#27023),(#27024,#27025),(#27026,#27027),(#27028,#27029),(#27030,#27031),
(#27032,#27033),(#27034,#27035),(#27036,#27037),(#27038,#27039),(#27040,
#27041),(#27042,#27043),(#27044,#27045),(#27046,#27047),(#27048,#27049),
(#27050,#27051),(#27052,#27053),(#27054,#27055),(#27056,#27057),(#27058,
#27059),(#27060,#27061),(#27062,#27063),(#27064,#27065),(#27066,#27067),
(#27068,#27069),(#27070,#27071),(#27072,#27073),(#27074,#27075),(#27076,
#27077),(#27078,#27079),(#27080,#27081),(#27082,#27083),(#27084,#27085),
(#27086,#27087),(#27088,#27089),(#27090,#27091),(#27092,#27093),(#27094,
#27095),(#27096,#27097),(#27098,#27099),(#27100,#27101),(#27102,#27103),
(#27104,#27105),(#27106,#27107),(#27108,#27109),(#27110,#27111),(#27112,
#27113),(#27114,#27115),(#27116,#27117),(#27118,#27119),(#27120,#27121),
(#27122,#27123),(#27124,#27125),(#27126,#27127),(#27128,#27129),(#27130,
#27131),(#27132,#27133),(#27134,#27135),(#27136,#27137),(#27138,#27139),
(#27140,#27141),(#27142,#27143),(#27144,#27145),(#27146,#27147),(#27148,
#27149),(#27150,#27151),(#27152,#27153),(#27154,#27155)),.UNSPECIFIED.,
 .F.,.F.,.F.)
B_SPLINE_SURFACE_WITH_KNOTS((6,1,1,1,1,1,1,1,1,1,1,1,1,1,1,1,1,1,1,1,1,
1,1,1,1,1,1,1,1,1,1,1,1,1,1,1,1,1,1,1,1,1,1,1,1,1,1,1,1,1,1,1,1,1,1,1,1,
1,1,1,1,1,1,1,1,6),(2,2),(-1.,-0.984615384615383,-0.969230769230768,-0.953846153846152,
-0.938461538461537,-0.923076923076922,-0.907692307692306,-0.892307692307691,
-0.876923076923076,-0.86153846153846,-0.846153846153845,-0.83076923076923,
-0.815384615384614,-0.799999999999999,-0.784615384615384,-0.769230769230768,
-0.753846153846153,-0.738461538461538,-0.723076923076922,-0.707692307692307,
-0.692307692307692,-0.676923076923076,-0.661538461538461,-0.646153846153846,
-0.63076923076923,-0.615384615384615,-0.6,-0.584615384615384,-0.569230769230769,
-0.553846153846154,-0.538461538461538,-0.523076923076923,-0.507692307692308,
-0.492307692307692,-0.476923076923077,-0.461538461538462,-0.446153846153846,
-0.430769230769231,-0.415384615384615,-0.4,-0.384615384615385,-0.369230769230769,
-0.353846153846154,-0.338461538461538,-0.323076923076923,-0.307692307692308,
-0.292307692307692,-0.276923076923077,-0.261538461538462,-0.246153846153846,
-0.230769230769231,-0.215384615384615,-0.2,-0.184615384615385,-0.169230769230769,
-0.153846153846154,-0.138461538461538,-0.123076923076923,-0.107692307692308,
-0.0923076923076923,-0.0769230769230769,-0.0615384615384615,-0.0461538461538462,
-0.0307692307692308,-0.0153846153846154,0.),(-1.,1.),.UNSPECIFIED.)
GEOMETRIC_REPRESENTATION_ITEM()
RATIONAL_B_SPLINE_SURFACE(((1.,1.),(1.,1.),(1.,1.),(1.,1.),(1.,1.),(1.,
1.),(1.,1.),(1.,1.),(1.,1.),(1.,1.),(1.,1.),(1.,1.),(1.,1.),(1.,1.),(1.,
1.),(1.,1.),(1.,1.),(1.,1.),(1.,1.),(1.,1.),(1.,1.),(1.,1.),(1.,1.),(1.,
1.),(1.,1.),(1.,1.),(1.,1.),(1.,1.),(1.,1.),(1.,1.),(1.,1.),(1.,1.),(1.,
1.),(1.,1.),(1.,1.),(1.,1.),(1.,1.),(1.,1.),(1.,1.),(1.,1.),(1.,1.),(1.,
1.),(1.,1.),(1.,1.),(1.,1.),(1.,1.),(1.,1.),(1.,1.),(1.,1.),(1.,1.),(1.,
1.),(1.,1.),(1.,1.),(1.,1.),(1.,1.),(1.,1.),(1.,1.),(1.,1.),(1.,1.),(1.,
1.),(1.,1.),(1.,1.),(1.,1.),(1.,1.),(1.,1.),(1.,1.),(1.,1.),(1.,1.),(1.,
1.),(1.,1.)))
REPRESENTATION_ITEM('')
SURFACE()
);
#27=(
BOUNDED_SURFACE()
B_SPLINE_SURFACE(5,1,((#27232,#27233),(#27234,#27235),(#27236,#27237),(#27238,
#27239),(#27240,#27241),(#27242,#27243),(#27244,#27245),(#27246,#27247),
(#27248,#27249),(#27250,#27251),(#27252,#27253),(#27254,#27255),(#27256,
#27257),(#27258,#27259),(#27260,#27261),(#27262,#27263),(#27264,#27265),
(#27266,#27267),(#27268,#27269),(#27270,#27271),(#27272,#27273),(#27274,
#27275),(#27276,#27277),(#27278,#27279),(#27280,#27281),(#27282,#27283),
(#27284,#27285),(#27286,#27287),(#27288,#27289),(#27290,#27291),(#27292,
#27293),(#27294,#27295),(#27296,#27297),(#27298,#27299),(#27300,#27301),
(#27302,#27303),(#27304,#27305),(#27306,#27307),(#27308,#27309),(#27310,
#27311),(#27312,#27313),(#27314,#27315),(#27316,#27317),(#27318,#27319),
(#27320,#27321),(#27322,#27323),(#27324,#27325),(#27326,#27327),(#27328,
#27329),(#27330,#27331),(#27332,#27333),(#27334,#27335),(#27336,#27337),
(#27338,#27339),(#27340,#27341),(#27342,#27343),(#27344,#27345),(#27346,
#27347),(#27348,#27349),(#27350,#27351),(#27352,#27353),(#27354,#27355),
(#27356,#27357),(#27358,#27359),(#27360,#27361),(#27362,#27363),(#27364,
#27365),(#27366,#27367),(#27368,#27369),(#27370,#27371)),.UNSPECIFIED.,
 .F.,.F.,.F.)
B_SPLINE_SURFACE_WITH_KNOTS((6,1,1,1,1,1,1,1,1,1,1,1,1,1,1,1,1,1,1,1,1,
1,1,1,1,1,1,1,1,1,1,1,1,1,1,1,1,1,1,1,1,1,1,1,1,1,1,1,1,1,1,1,1,1,1,1,1,
1,1,1,1,1,1,1,1,6),(2,2),(-1.,-0.984615384615383,-0.969230769230768,-0.953846153846152,
-0.938461538461537,-0.923076923076922,-0.907692307692306,-0.892307692307691,
-0.876923076923076,-0.86153846153846,-0.846153846153845,-0.83076923076923,
-0.815384615384614,-0.799999999999999,-0.784615384615384,-0.769230769230768,
-0.753846153846153,-0.738461538461538,-0.723076923076922,-0.707692307692307,
-0.692307692307692,-0.676923076923076,-0.661538461538461,-0.646153846153846,
-0.63076923076923,-0.615384615384615,-0.6,-0.584615384615384,-0.569230769230769,
-0.553846153846154,-0.538461538461538,-0.523076923076923,-0.507692307692308,
-0.492307692307692,-0.476923076923077,-0.461538461538462,-0.446153846153846,
-0.430769230769231,-0.415384615384615,-0.4,-0.384615384615385,-0.369230769230769,
-0.353846153846154,-0.338461538461538,-0.323076923076923,-0.307692307692308,
-0.292307692307692,-0.276923076923077,-0.261538461538462,-0.246153846153846,
-0.230769230769231,-0.215384615384615,-0.2,-0.184615384615385,-0.169230769230769,
-0.153846153846154,-0.138461538461538,-0.123076923076923,-0.107692307692308,
-0.0923076923076923,-0.0769230769230769,-0.0615384615384615,-0.0461538461538462,
-0.0307692307692308,-0.0153846153846154,0.),(-1.,1.),.UNSPECIFIED.)
GEOMETRIC_REPRESENTATION_ITEM()
RATIONAL_B_SPLINE_SURFACE(((1.,1.),(1.,1.),(1.,1.),(1.,1.),(1.,1.),(1.,
1.),(1.,1.),(1.,1.),(1.,1.),(1.,1.),(1.,1.),(1.,1.),(1.,1.),(1.,1.),(1.,
1.),(1.,1.),(1.,1.),(1.,1.),(1.,1.),(1.,1.),(1.,1.),(1.,1.),(1.,1.),(1.,
1.),(1.,1.),(1.,1.),(1.,1.),(1.,1.),(1.,1.),(1.,1.),(1.,1.),(1.,1.),(1.,
1.),(1.,1.),(1.,1.),(1.,1.),(1.,1.),(1.,1.),(1.,1.),(1.,1.),(1.,1.),(1.,
1.),(1.,1.),(1.,1.),(1.,1.),(1.,1.),(1.,1.),(1.,1.),(1.,1.),(1.,1.),(1.,
1.),(1.,1.),(1.,1.),(1.,1.),(1.,1.),(1.,1.),(1.,1.),(1.,1.),(1.,1.),(1.,
1.),(1.,1.),(1.,1.),(1.,1.),(1.,1.),(1.,1.),(1.,1.),(1.,1.),(1.,1.),(1.,
1.),(1.,1.)))
REPRESENTATION_ITEM('')
SURFACE()
);
#28=(
BOUNDED_SURFACE()
B_SPLINE_SURFACE(5,1,((#27448,#27449),(#27450,#27451),(#27452,#27453),(#27454,
#27455),(#27456,#27457),(#27458,#27459),(#27460,#27461),(#27462,#27463),
(#27464,#27465),(#27466,#27467),(#27468,#27469),(#27470,#27471),(#27472,
#27473),(#27474,#27475),(#27476,#27477),(#27478,#27479),(#27480,#27481),
(#27482,#27483),(#27484,#27485),(#27486,#27487),(#27488,#27489),(#27490,
#27491),(#27492,#27493),(#27494,#27495),(#27496,#27497),(#27498,#27499),
(#27500,#27501),(#27502,#27503),(#27504,#27505),(#27506,#27507),(#27508,
#27509),(#27510,#27511),(#27512,#27513),(#27514,#27515),(#27516,#27517),
(#27518,#27519),(#27520,#27521),(#27522,#27523),(#27524,#27525),(#27526,
#27527),(#27528,#27529),(#27530,#27531),(#27532,#27533),(#27534,#27535),
(#27536,#27537),(#27538,#27539),(#27540,#27541),(#27542,#27543),(#27544,
#27545),(#27546,#27547),(#27548,#27549),(#27550,#27551),(#27552,#27553),
(#27554,#27555),(#27556,#27557),(#27558,#27559),(#27560,#27561),(#27562,
#27563),(#27564,#27565),(#27566,#27567),(#27568,#27569),(#27570,#27571),
(#27572,#27573),(#27574,#27575),(#27576,#27577),(#27578,#27579),(#27580,
#27581),(#27582,#27583),(#27584,#27585),(#27586,#27587)),.UNSPECIFIED.,
 .F.,.F.,.F.)
B_SPLINE_SURFACE_WITH_KNOTS((6,1,1,1,1,1,1,1,1,1,1,1,1,1,1,1,1,1,1,1,1,
1,1,1,1,1,1,1,1,1,1,1,1,1,1,1,1,1,1,1,1,1,1,1,1,1,1,1,1,1,1,1,1,1,1,1,1,
1,1,1,1,1,1,1,1,6),(2,2),(-1.,-0.984615384615383,-0.969230769230768,-0.953846153846152,
-0.938461538461537,-0.923076923076922,-0.907692307692306,-0.892307692307691,
-0.876923076923076,-0.86153846153846,-0.846153846153845,-0.83076923076923,
-0.815384615384614,-0.799999999999999,-0.784615384615384,-0.769230769230768,
-0.753846153846153,-0.738461538461538,-0.723076923076922,-0.707692307692307,
-0.692307692307692,-0.676923076923076,-0.661538461538461,-0.646153846153846,
-0.63076923076923,-0.615384615384615,-0.6,-0.584615384615384,-0.569230769230769,
-0.553846153846154,-0.538461538461538,-0.523076923076923,-0.507692307692308,
-0.492307692307692,-0.476923076923077,-0.461538461538462,-0.446153846153846,
-0.430769230769231,-0.415384615384615,-0.4,-0.384615384615385,-0.369230769230769,
-0.353846153846154,-0.338461538461538,-0.323076923076923,-0.307692307692308,
-0.292307692307692,-0.276923076923077,-0.261538461538462,-0.246153846153846,
-0.230769230769231,-0.215384615384615,-0.2,-0.184615384615385,-0.169230769230769,
-0.153846153846154,-0.138461538461538,-0.123076923076923,-0.107692307692308,
-0.0923076923076923,-0.0769230769230769,-0.0615384615384615,-0.0461538461538462,
-0.0307692307692308,-0.0153846153846154,0.),(-1.,1.),.UNSPECIFIED.)
GEOMETRIC_REPRESENTATION_ITEM()
RATIONAL_B_SPLINE_SURFACE(((1.,1.),(1.,1.),(1.,1.),(1.,1.),(1.,1.),(1.,
1.),(1.,1.),(1.,1.),(1.,1.),(1.,1.),(1.,1.),(1.,1.),(1.,1.),(1.,1.),(1.,
1.),(1.,1.),(1.,1.),(1.,1.),(1.,1.),(1.,1.),(1.,1.),(1.,1.),(1.,1.),(1.,
1.),(1.,1.),(1.,1.),(1.,1.),(1.,1.),(1.,1.),(1.,1.),(1.,1.),(1.,1.),(1.,
1.),(1.,1.),(1.,1.),(1.,1.),(1.,1.),(1.,1.),(1.,1.),(1.,1.),(1.,1.),(1.,
1.),(1.,1.),(1.,1.),(1.,1.),(1.,1.),(1.,1.),(1.,1.),(1.,1.),(1.,1.),(1.,
1.),(1.,1.),(1.,1.),(1.,1.),(1.,1.),(1.,1.),(1.,1.),(1.,1.),(1.,1.),(1.,
1.),(1.,1.),(1.,1.),(1.,1.),(1.,1.),(1.,1.),(1.,1.),(1.,1.),(1.,1.),(1.,
1.),(1.,1.)))
REPRESENTATION_ITEM('')
SURFACE()
);
#29=(
BOUNDED_SURFACE()
B_SPLINE_SURFACE(5,1,((#27664,#27665),(#27666,#27667),(#27668,#27669),(#27670,
#27671),(#27672,#27673),(#27674,#27675),(#27676,#27677),(#27678,#27679),
(#27680,#27681),(#27682,#27683),(#27684,#27685),(#27686,#27687),(#27688,
#27689),(#27690,#27691),(#27692,#27693),(#27694,#27695),(#27696,#27697),
(#27698,#27699),(#27700,#27701),(#27702,#27703),(#27704,#27705),(#27706,
#27707),(#27708,#27709),(#27710,#27711),(#27712,#27713),(#27714,#27715),
(#27716,#27717),(#27718,#27719),(#27720,#27721),(#27722,#27723),(#27724,
#27725),(#27726,#27727),(#27728,#27729),(#27730,#27731),(#27732,#27733),
(#27734,#27735),(#27736,#27737),(#27738,#27739),(#27740,#27741),(#27742,
#27743),(#27744,#27745),(#27746,#27747),(#27748,#27749),(#27750,#27751),
(#27752,#27753),(#27754,#27755),(#27756,#27757),(#27758,#27759),(#27760,
#27761),(#27762,#27763),(#27764,#27765),(#27766,#27767),(#27768,#27769),
(#27770,#27771),(#27772,#27773),(#27774,#27775),(#27776,#27777),(#27778,
#27779),(#27780,#27781),(#27782,#27783),(#27784,#27785),(#27786,#27787),
(#27788,#27789),(#27790,#27791),(#27792,#27793),(#27794,#27795),(#27796,
#27797),(#27798,#27799),(#27800,#27801),(#27802,#27803)),.UNSPECIFIED.,
 .F.,.F.,.F.)
B_SPLINE_SURFACE_WITH_KNOTS((6,1,1,1,1,1,1,1,1,1,1,1,1,1,1,1,1,1,1,1,1,
1,1,1,1,1,1,1,1,1,1,1,1,1,1,1,1,1,1,1,1,1,1,1,1,1,1,1,1,1,1,1,1,1,1,1,1,
1,1,1,1,1,1,1,1,6),(2,2),(-1.,-0.984615384615383,-0.969230769230768,-0.953846153846152,
-0.938461538461537,-0.923076923076922,-0.907692307692306,-0.892307692307691,
-0.876923076923076,-0.86153846153846,-0.846153846153845,-0.83076923076923,
-0.815384615384614,-0.799999999999999,-0.784615384615384,-0.769230769230768,
-0.753846153846153,-0.738461538461538,-0.723076923076922,-0.707692307692307,
-0.692307692307692,-0.676923076923076,-0.661538461538461,-0.646153846153846,
-0.63076923076923,-0.615384615384615,-0.6,-0.584615384615384,-0.569230769230769,
-0.553846153846154,-0.538461538461538,-0.523076923076923,-0.507692307692308,
-0.492307692307692,-0.476923076923077,-0.461538461538462,-0.446153846153846,
-0.430769230769231,-0.415384615384615,-0.4,-0.384615384615385,-0.369230769230769,
-0.353846153846154,-0.338461538461538,-0.323076923076923,-0.307692307692308,
-0.292307692307692,-0.276923076923077,-0.261538461538462,-0.246153846153846,
-0.230769230769231,-0.215384615384615,-0.2,-0.184615384615385,-0.169230769230769,
-0.153846153846154,-0.138461538461538,-0.123076923076923,-0.107692307692308,
-0.0923076923076923,-0.0769230769230769,-0.0615384615384615,-0.0461538461538462,
-0.0307692307692308,-0.0153846153846154,0.),(-1.,1.),.UNSPECIFIED.)
GEOMETRIC_REPRESENTATION_ITEM()
RATIONAL_B_SPLINE_SURFACE(((1.,1.),(1.,1.),(1.,1.),(1.,1.),(1.,1.),(1.,
1.),(1.,1.),(1.,1.),(1.,1.),(1.,1.),(1.,1.),(1.,1.),(1.,1.),(1.,1.),(1.,
1.),(1.,1.),(1.,1.),(1.,1.),(1.,1.),(1.,1.),(1.,1.),(1.,1.),(1.,1.),(1.,
1.),(1.,1.),(1.,1.),(1.,1.),(1.,1.),(1.,1.),(1.,1.),(1.,1.),(1.,1.),(1.,
1.),(1.,1.),(1.,1.),(1.,1.),(1.,1.),(1.,1.),(1.,1.),(1.,1.),(1.,1.),(1.,
1.),(1.,1.),(1.,1.),(1.,1.),(1.,1.),(1.,1.),(1.,1.),(1.,1.),(1.,1.),(1.,
1.),(1.,1.),(1.,1.),(1.,1.),(1.,1.),(1.,1.),(1.,1.),(1.,1.),(1.,1.),(1.,
1.),(1.,1.),(1.,1.),(1.,1.),(1.,1.),(1.,1.),(1.,1.),(1.,1.),(1.,1.),(1.,
1.),(1.,1.)))
REPRESENTATION_ITEM('')
SURFACE()
);
#30=(
BOUNDED_SURFACE()
B_SPLINE_SURFACE(5,1,((#27880,#27881),(#27882,#27883),(#27884,#27885),(#27886,
#27887),(#27888,#27889),(#27890,#27891),(#27892,#27893),(#27894,#27895),
(#27896,#27897),(#27898,#27899),(#27900,#27901),(#27902,#27903),(#27904,
#27905),(#27906,#27907),(#27908,#27909),(#27910,#27911),(#27912,#27913),
(#27914,#27915),(#27916,#27917),(#27918,#27919),(#27920,#27921),(#27922,
#27923),(#27924,#27925),(#27926,#27927),(#27928,#27929),(#27930,#27931),
(#27932,#27933),(#27934,#27935),(#27936,#27937),(#27938,#27939),(#27940,
#27941),(#27942,#27943),(#27944,#27945),(#27946,#27947),(#27948,#27949),
(#27950,#27951),(#27952,#27953),(#27954,#27955),(#27956,#27957),(#27958,
#27959),(#27960,#27961),(#27962,#27963),(#27964,#27965),(#27966,#27967),
(#27968,#27969),(#27970,#27971),(#27972,#27973),(#27974,#27975),(#27976,
#27977),(#27978,#27979),(#27980,#27981),(#27982,#27983),(#27984,#27985),
(#27986,#27987),(#27988,#27989),(#27990,#27991),(#27992,#27993),(#27994,
#27995),(#27996,#27997),(#27998,#27999),(#28000,#28001),(#28002,#28003),
(#28004,#28005),(#28006,#28007),(#28008,#28009),(#28010,#28011),(#28012,
#28013),(#28014,#28015),(#28016,#28017),(#28018,#28019)),.UNSPECIFIED.,
 .F.,.F.,.F.)
B_SPLINE_SURFACE_WITH_KNOTS((6,1,1,1,1,1,1,1,1,1,1,1,1,1,1,1,1,1,1,1,1,
1,1,1,1,1,1,1,1,1,1,1,1,1,1,1,1,1,1,1,1,1,1,1,1,1,1,1,1,1,1,1,1,1,1,1,1,
1,1,1,1,1,1,1,1,6),(2,2),(-1.,-0.984615384615383,-0.969230769230768,-0.953846153846152,
-0.938461538461537,-0.923076923076922,-0.907692307692306,-0.892307692307691,
-0.876923076923076,-0.86153846153846,-0.846153846153845,-0.83076923076923,
-0.815384615384614,-0.799999999999999,-0.784615384615384,-0.769230769230768,
-0.753846153846153,-0.738461538461538,-0.723076923076922,-0.707692307692307,
-0.692307692307692,-0.676923076923076,-0.661538461538461,-0.646153846153846,
-0.63076923076923,-0.615384615384615,-0.6,-0.584615384615384,-0.569230769230769,
-0.553846153846154,-0.538461538461538,-0.523076923076923,-0.507692307692308,
-0.492307692307692,-0.476923076923077,-0.461538461538462,-0.446153846153846,
-0.430769230769231,-0.415384615384615,-0.4,-0.384615384615385,-0.369230769230769,
-0.353846153846154,-0.338461538461538,-0.323076923076923,-0.307692307692308,
-0.292307692307692,-0.276923076923077,-0.261538461538462,-0.246153846153846,
-0.230769230769231,-0.215384615384615,-0.2,-0.184615384615385,-0.169230769230769,
-0.153846153846154,-0.138461538461538,-0.123076923076923,-0.107692307692308,
-0.0923076923076923,-0.0769230769230769,-0.0615384615384615,-0.0461538461538462,
-0.0307692307692308,-0.0153846153846154,0.),(-1.,1.),.UNSPECIFIED.)
GEOMETRIC_REPRESENTATION_ITEM()
RATIONAL_B_SPLINE_SURFACE(((1.,1.),(1.,1.),(1.,1.),(1.,1.),(1.,1.),(1.,
1.),(1.,1.),(1.,1.),(1.,1.),(1.,1.),(1.,1.),(1.,1.),(1.,1.),(1.,1.),(1.,
1.),(1.,1.),(1.,1.),(1.,1.),(1.,1.),(1.,1.),(1.,1.),(1.,1.),(1.,1.),(1.,
1.),(1.,1.),(1.,1.),(1.,1.),(1.,1.),(1.,1.),(1.,1.),(1.,1.),(1.,1.),(1.,
1.),(1.,1.),(1.,1.),(1.,1.),(1.,1.),(1.,1.),(1.,1.),(1.,1.),(1.,1.),(1.,
1.),(1.,1.),(1.,1.),(1.,1.),(1.,1.),(1.,1.),(1.,1.),(1.,1.),(1.,1.),(1.,
1.),(1.,1.),(1.,1.),(1.,1.),(1.,1.),(1.,1.),(1.,1.),(1.,1.),(1.,1.),(1.,
1.),(1.,1.),(1.,1.),(1.,1.),(1.,1.),(1.,1.),(1.,1.),(1.,1.),(1.,1.),(1.,
1.),(1.,1.)))
REPRESENTATION_ITEM('')
SURFACE()
);
#31=(
BOUNDED_SURFACE()
B_SPLINE_SURFACE(5,1,((#28096,#28097),(#28098,#28099),(#28100,#28101),(#28102,
#28103),(#28104,#28105),(#28106,#28107),(#28108,#28109),(#28110,#28111),
(#28112,#28113),(#28114,#28115),(#28116,#28117),(#28118,#28119),(#28120,
#28121),(#28122,#28123),(#28124,#28125),(#28126,#28127),(#28128,#28129),
(#28130,#28131),(#28132,#28133),(#28134,#28135),(#28136,#28137),(#28138,
#28139),(#28140,#28141),(#28142,#28143),(#28144,#28145),(#28146,#28147),
(#28148,#28149),(#28150,#28151),(#28152,#28153),(#28154,#28155),(#28156,
#28157),(#28158,#28159),(#28160,#28161),(#28162,#28163),(#28164,#28165),
(#28166,#28167),(#28168,#28169),(#28170,#28171),(#28172,#28173),(#28174,
#28175),(#28176,#28177),(#28178,#28179),(#28180,#28181),(#28182,#28183),
(#28184,#28185),(#28186,#28187),(#28188,#28189),(#28190,#28191),(#28192,
#28193),(#28194,#28195),(#28196,#28197),(#28198,#28199),(#28200,#28201),
(#28202,#28203),(#28204,#28205),(#28206,#28207),(#28208,#28209),(#28210,
#28211),(#28212,#28213),(#28214,#28215),(#28216,#28217),(#28218,#28219),
(#28220,#28221),(#28222,#28223),(#28224,#28225),(#28226,#28227),(#28228,
#28229),(#28230,#28231),(#28232,#28233),(#28234,#28235)),.UNSPECIFIED.,
 .F.,.F.,.F.)
B_SPLINE_SURFACE_WITH_KNOTS((6,1,1,1,1,1,1,1,1,1,1,1,1,1,1,1,1,1,1,1,1,
1,1,1,1,1,1,1,1,1,1,1,1,1,1,1,1,1,1,1,1,1,1,1,1,1,1,1,1,1,1,1,1,1,1,1,1,
1,1,1,1,1,1,1,1,6),(2,2),(-1.,-0.984615384615383,-0.969230769230768,-0.953846153846152,
-0.938461538461537,-0.923076923076922,-0.907692307692306,-0.892307692307691,
-0.876923076923076,-0.86153846153846,-0.846153846153845,-0.83076923076923,
-0.815384615384614,-0.799999999999999,-0.784615384615384,-0.769230769230768,
-0.753846153846153,-0.738461538461538,-0.723076923076922,-0.707692307692307,
-0.692307692307692,-0.676923076923076,-0.661538461538461,-0.646153846153846,
-0.63076923076923,-0.615384615384615,-0.6,-0.584615384615384,-0.569230769230769,
-0.553846153846154,-0.538461538461538,-0.523076923076923,-0.507692307692308,
-0.492307692307692,-0.476923076923077,-0.461538461538462,-0.446153846153846,
-0.430769230769231,-0.415384615384615,-0.4,-0.384615384615385,-0.369230769230769,
-0.353846153846154,-0.338461538461538,-0.323076923076923,-0.307692307692308,
-0.292307692307692,-0.276923076923077,-0.261538461538462,-0.246153846153846,
-0.230769230769231,-0.215384615384615,-0.2,-0.184615384615385,-0.169230769230769,
-0.153846153846154,-0.138461538461538,-0.123076923076923,-0.107692307692308,
-0.0923076923076923,-0.0769230769230769,-0.0615384615384615,-0.0461538461538462,
-0.0307692307692308,-0.0153846153846154,0.),(-1.,1.),.UNSPECIFIED.)
GEOMETRIC_REPRESENTATION_ITEM()
RATIONAL_B_SPLINE_SURFACE(((1.,1.),(1.,1.),(1.,1.),(1.,1.),(1.,1.),(1.,
1.),(1.,1.),(1.,1.),(1.,1.),(1.,1.),(1.,1.),(1.,1.),(1.,1.),(1.,1.),(1.,
1.),(1.,1.),(1.,1.),(1.,1.),(1.,1.),(1.,1.),(1.,1.),(1.,1.),(1.,1.),(1.,
1.),(1.,1.),(1.,1.),(1.,1.),(1.,1.),(1.,1.),(1.,1.),(1.,1.),(1.,1.),(1.,
1.),(1.,1.),(1.,1.),(1.,1.),(1.,1.),(1.,1.),(1.,1.),(1.,1.),(1.,1.),(1.,
1.),(1.,1.),(1.,1.),(1.,1.),(1.,1.),(1.,1.),(1.,1.),(1.,1.),(1.,1.),(1.,
1.),(1.,1.),(1.,1.),(1.,1.),(1.,1.),(1.,1.),(1.,1.),(1.,1.),(1.,1.),(1.,
1.),(1.,1.),(1.,1.),(1.,1.),(1.,1.),(1.,1.),(1.,1.),(1.,1.),(1.,1.),(1.,
1.),(1.,1.)))
REPRESENTATION_ITEM('')
SURFACE()
);
#32=(
BOUNDED_SURFACE()
B_SPLINE_SURFACE(5,1,((#28312,#28313),(#28314,#28315),(#28316,#28317),(#28318,
#28319),(#28320,#28321),(#28322,#28323),(#28324,#28325),(#28326,#28327),
(#28328,#28329),(#28330,#28331),(#28332,#28333),(#28334,#28335),(#28336,
#28337),(#28338,#28339),(#28340,#28341),(#28342,#28343),(#28344,#28345),
(#28346,#28347),(#28348,#28349),(#28350,#28351),(#28352,#28353),(#28354,
#28355),(#28356,#28357),(#28358,#28359),(#28360,#28361),(#28362,#28363),
(#28364,#28365),(#28366,#28367),(#28368,#28369),(#28370,#28371),(#28372,
#28373),(#28374,#28375),(#28376,#28377),(#28378,#28379),(#28380,#28381),
(#28382,#28383),(#28384,#28385),(#28386,#28387),(#28388,#28389),(#28390,
#28391),(#28392,#28393),(#28394,#28395),(#28396,#28397),(#28398,#28399),
(#28400,#28401),(#28402,#28403),(#28404,#28405),(#28406,#28407),(#28408,
#28409),(#28410,#28411),(#28412,#28413),(#28414,#28415),(#28416,#28417),
(#28418,#28419),(#28420,#28421),(#28422,#28423),(#28424,#28425),(#28426,
#28427),(#28428,#28429),(#28430,#28431),(#28432,#28433),(#28434,#28435),
(#28436,#28437),(#28438,#28439),(#28440,#28441),(#28442,#28443),(#28444,
#28445),(#28446,#28447),(#28448,#28449),(#28450,#28451)),.UNSPECIFIED.,
 .F.,.F.,.F.)
B_SPLINE_SURFACE_WITH_KNOTS((6,1,1,1,1,1,1,1,1,1,1,1,1,1,1,1,1,1,1,1,1,
1,1,1,1,1,1,1,1,1,1,1,1,1,1,1,1,1,1,1,1,1,1,1,1,1,1,1,1,1,1,1,1,1,1,1,1,
1,1,1,1,1,1,1,1,6),(2,2),(-1.,-0.984615384615383,-0.969230769230768,-0.953846153846152,
-0.938461538461537,-0.923076923076922,-0.907692307692306,-0.892307692307691,
-0.876923076923076,-0.86153846153846,-0.846153846153845,-0.83076923076923,
-0.815384615384614,-0.799999999999999,-0.784615384615384,-0.769230769230768,
-0.753846153846153,-0.738461538461538,-0.723076923076922,-0.707692307692307,
-0.692307692307692,-0.676923076923076,-0.661538461538461,-0.646153846153846,
-0.63076923076923,-0.615384615384615,-0.6,-0.584615384615384,-0.569230769230769,
-0.553846153846154,-0.538461538461538,-0.523076923076923,-0.507692307692308,
-0.492307692307692,-0.476923076923077,-0.461538461538462,-0.446153846153846,
-0.430769230769231,-0.415384615384615,-0.4,-0.384615384615385,-0.369230769230769,
-0.353846153846154,-0.338461538461538,-0.323076923076923,-0.307692307692308,
-0.292307692307692,-0.276923076923077,-0.261538461538462,-0.246153846153846,
-0.230769230769231,-0.215384615384615,-0.2,-0.184615384615385,-0.169230769230769,
-0.153846153846154,-0.138461538461538,-0.123076923076923,-0.107692307692308,
-0.0923076923076923,-0.0769230769230769,-0.0615384615384615,-0.0461538461538462,
-0.0307692307692308,-0.0153846153846154,0.),(-1.,1.),.UNSPECIFIED.)
GEOMETRIC_REPRESENTATION_ITEM()
RATIONAL_B_SPLINE_SURFACE(((1.,1.),(1.,1.),(1.,1.),(1.,1.),(1.,1.),(1.,
1.),(1.,1.),(1.,1.),(1.,1.),(1.,1.),(1.,1.),(1.,1.),(1.,1.),(1.,1.),(1.,
1.),(1.,1.),(1.,1.),(1.,1.),(1.,1.),(1.,1.),(1.,1.),(1.,1.),(1.,1.),(1.,
1.),(1.,1.),(1.,1.),(1.,1.),(1.,1.),(1.,1.),(1.,1.),(1.,1.),(1.,1.),(1.,
1.),(1.,1.),(1.,1.),(1.,1.),(1.,1.),(1.,1.),(1.,1.),(1.,1.),(1.,1.),(1.,
1.),(1.,1.),(1.,1.),(1.,1.),(1.,1.),(1.,1.),(1.,1.),(1.,1.),(1.,1.),(1.,
1.),(1.,1.),(1.,1.),(1.,1.),(1.,1.),(1.,1.),(1.,1.),(1.,1.),(1.,1.),(1.,
1.),(1.,1.),(1.,1.),(1.,1.),(1.,1.),(1.,1.),(1.,1.),(1.,1.),(1.,1.),(1.,
1.),(1.,1.)))
REPRESENTATION_ITEM('')
SURFACE()
);
#33=(
BOUNDED_SURFACE()
B_SPLINE_SURFACE(5,1,((#28528,#28529),(#28530,#28531),(#28532,#28533),(#28534,
#28535),(#28536,#28537),(#28538,#28539),(#28540,#28541),(#28542,#28543),
(#28544,#28545),(#28546,#28547),(#28548,#28549),(#28550,#28551),(#28552,
#28553),(#28554,#28555),(#28556,#28557),(#28558,#28559),(#28560,#28561),
(#28562,#28563),(#28564,#28565),(#28566,#28567),(#28568,#28569),(#28570,
#28571),(#28572,#28573),(#28574,#28575),(#28576,#28577),(#28578,#28579),
(#28580,#28581),(#28582,#28583),(#28584,#28585),(#28586,#28587),(#28588,
#28589),(#28590,#28591),(#28592,#28593),(#28594,#28595),(#28596,#28597),
(#28598,#28599),(#28600,#28601),(#28602,#28603),(#28604,#28605),(#28606,
#28607),(#28608,#28609),(#28610,#28611),(#28612,#28613),(#28614,#28615),
(#28616,#28617),(#28618,#28619),(#28620,#28621),(#28622,#28623),(#28624,
#28625),(#28626,#28627),(#28628,#28629),(#28630,#28631),(#28632,#28633),
(#28634,#28635),(#28636,#28637),(#28638,#28639),(#28640,#28641),(#28642,
#28643),(#28644,#28645),(#28646,#28647),(#28648,#28649),(#28650,#28651),
(#28652,#28653),(#28654,#28655),(#28656,#28657),(#28658,#28659),(#28660,
#28661),(#28662,#28663),(#28664,#28665),(#28666,#28667)),.UNSPECIFIED.,
 .F.,.F.,.F.)
B_SPLINE_SURFACE_WITH_KNOTS((6,1,1,1,1,1,1,1,1,1,1,1,1,1,1,1,1,1,1,1,1,
1,1,1,1,1,1,1,1,1,1,1,1,1,1,1,1,1,1,1,1,1,1,1,1,1,1,1,1,1,1,1,1,1,1,1,1,
1,1,1,1,1,1,1,1,6),(2,2),(-1.,-0.984615384615383,-0.969230769230768,-0.953846153846152,
-0.938461538461537,-0.923076923076922,-0.907692307692306,-0.892307692307691,
-0.876923076923076,-0.86153846153846,-0.846153846153845,-0.83076923076923,
-0.815384615384614,-0.799999999999999,-0.784615384615384,-0.769230769230768,
-0.753846153846153,-0.738461538461538,-0.723076923076922,-0.707692307692307,
-0.692307692307692,-0.676923076923076,-0.661538461538461,-0.646153846153846,
-0.63076923076923,-0.615384615384615,-0.6,-0.584615384615384,-0.569230769230769,
-0.553846153846154,-0.538461538461538,-0.523076923076923,-0.507692307692308,
-0.492307692307692,-0.476923076923077,-0.461538461538462,-0.446153846153846,
-0.430769230769231,-0.415384615384615,-0.4,-0.384615384615385,-0.369230769230769,
-0.353846153846154,-0.338461538461538,-0.323076923076923,-0.307692307692308,
-0.292307692307692,-0.276923076923077,-0.261538461538462,-0.246153846153846,
-0.230769230769231,-0.215384615384615,-0.2,-0.184615384615385,-0.169230769230769,
-0.153846153846154,-0.138461538461538,-0.123076923076923,-0.107692307692308,
-0.0923076923076923,-0.0769230769230769,-0.0615384615384615,-0.0461538461538462,
-0.0307692307692308,-0.0153846153846154,0.),(-1.,1.),.UNSPECIFIED.)
GEOMETRIC_REPRESENTATION_ITEM()
RATIONAL_B_SPLINE_SURFACE(((1.,1.),(1.,1.),(1.,1.),(1.,1.),(1.,1.),(1.,
1.),(1.,1.),(1.,1.),(1.,1.),(1.,1.),(1.,1.),(1.,1.),(1.,1.),(1.,1.),(1.,
1.),(1.,1.),(1.,1.),(1.,1.),(1.,1.),(1.,1.),(1.,1.),(1.,1.),(1.,1.),(1.,
1.),(1.,1.),(1.,1.),(1.,1.),(1.,1.),(1.,1.),(1.,1.),(1.,1.),(1.,1.),(1.,
1.),(1.,1.),(1.,1.),(1.,1.),(1.,1.),(1.,1.),(1.,1.),(1.,1.),(1.,1.),(1.,
1.),(1.,1.),(1.,1.),(1.,1.),(1.,1.),(1.,1.),(1.,1.),(1.,1.),(1.,1.),(1.,
1.),(1.,1.),(1.,1.),(1.,1.),(1.,1.),(1.,1.),(1.,1.),(1.,1.),(1.,1.),(1.,
1.),(1.,1.),(1.,1.),(1.,1.),(1.,1.),(1.,1.),(1.,1.),(1.,1.),(1.,1.),(1.,
1.),(1.,1.)))
REPRESENTATION_ITEM('')
SURFACE()
);
#34=(
BOUNDED_SURFACE()
B_SPLINE_SURFACE(5,1,((#28744,#28745),(#28746,#28747),(#28748,#28749),(#28750,
#28751),(#28752,#28753),(#28754,#28755),(#28756,#28757),(#28758,#28759),
(#28760,#28761),(#28762,#28763),(#28764,#28765),(#28766,#28767),(#28768,
#28769),(#28770,#28771),(#28772,#28773),(#28774,#28775),(#28776,#28777),
(#28778,#28779),(#28780,#28781),(#28782,#28783),(#28784,#28785),(#28786,
#28787),(#28788,#28789),(#28790,#28791),(#28792,#28793),(#28794,#28795),
(#28796,#28797),(#28798,#28799),(#28800,#28801),(#28802,#28803),(#28804,
#28805),(#28806,#28807),(#28808,#28809),(#28810,#28811),(#28812,#28813),
(#28814,#28815),(#28816,#28817),(#28818,#28819),(#28820,#28821),(#28822,
#28823),(#28824,#28825),(#28826,#28827),(#28828,#28829),(#28830,#28831),
(#28832,#28833),(#28834,#28835),(#28836,#28837),(#28838,#28839),(#28840,
#28841),(#28842,#28843),(#28844,#28845),(#28846,#28847),(#28848,#28849),
(#28850,#28851),(#28852,#28853),(#28854,#28855),(#28856,#28857),(#28858,
#28859),(#28860,#28861),(#28862,#28863),(#28864,#28865),(#28866,#28867),
(#28868,#28869),(#28870,#28871),(#28872,#28873),(#28874,#28875),(#28876,
#28877),(#28878,#28879),(#28880,#28881),(#28882,#28883)),.UNSPECIFIED.,
 .F.,.F.,.F.)
B_SPLINE_SURFACE_WITH_KNOTS((6,1,1,1,1,1,1,1,1,1,1,1,1,1,1,1,1,1,1,1,1,
1,1,1,1,1,1,1,1,1,1,1,1,1,1,1,1,1,1,1,1,1,1,1,1,1,1,1,1,1,1,1,1,1,1,1,1,
1,1,1,1,1,1,1,1,6),(2,2),(-1.,-0.984615384615383,-0.969230769230768,-0.953846153846152,
-0.938461538461537,-0.923076923076922,-0.907692307692306,-0.892307692307691,
-0.876923076923076,-0.86153846153846,-0.846153846153845,-0.83076923076923,
-0.815384615384614,-0.799999999999999,-0.784615384615384,-0.769230769230768,
-0.753846153846153,-0.738461538461538,-0.723076923076922,-0.707692307692307,
-0.692307692307692,-0.676923076923076,-0.661538461538461,-0.646153846153846,
-0.63076923076923,-0.615384615384615,-0.6,-0.584615384615384,-0.569230769230769,
-0.553846153846154,-0.538461538461538,-0.523076923076923,-0.507692307692308,
-0.492307692307692,-0.476923076923077,-0.461538461538462,-0.446153846153846,
-0.430769230769231,-0.415384615384615,-0.4,-0.384615384615385,-0.369230769230769,
-0.353846153846154,-0.338461538461538,-0.323076923076923,-0.307692307692308,
-0.292307692307692,-0.276923076923077,-0.261538461538462,-0.246153846153846,
-0.230769230769231,-0.215384615384615,-0.2,-0.184615384615385,-0.169230769230769,
-0.153846153846154,-0.138461538461538,-0.123076923076923,-0.107692307692308,
-0.0923076923076923,-0.0769230769230769,-0.0615384615384615,-0.0461538461538462,
-0.0307692307692308,-0.0153846153846154,0.),(-1.,1.),.UNSPECIFIED.)
GEOMETRIC_REPRESENTATION_ITEM()
RATIONAL_B_SPLINE_SURFACE(((1.,1.),(1.,1.),(1.,1.),(1.,1.),(1.,1.),(1.,
1.),(1.,1.),(1.,1.),(1.,1.),(1.,1.),(1.,1.),(1.,1.),(1.,1.),(1.,1.),(1.,
1.),(1.,1.),(1.,1.),(1.,1.),(1.,1.),(1.,1.),(1.,1.),(1.,1.),(1.,1.),(1.,
1.),(1.,1.),(1.,1.),(1.,1.),(1.,1.),(1.,1.),(1.,1.),(1.,1.),(1.,1.),(1.,
1.),(1.,1.),(1.,1.),(1.,1.),(1.,1.),(1.,1.),(1.,1.),(1.,1.),(1.,1.),(1.,
1.),(1.,1.),(1.,1.),(1.,1.),(1.,1.),(1.,1.),(1.,1.),(1.,1.),(1.,1.),(1.,
1.),(1.,1.),(1.,1.),(1.,1.),(1.,1.),(1.,1.),(1.,1.),(1.,1.),(1.,1.),(1.,
1.),(1.,1.),(1.,1.),(1.,1.),(1.,1.),(1.,1.),(1.,1.),(1.,1.),(1.,1.),(1.,
1.),(1.,1.)))
REPRESENTATION_ITEM('')
SURFACE()
);
#35=(
BOUNDED_SURFACE()
B_SPLINE_SURFACE(5,1,((#28960,#28961),(#28962,#28963),(#28964,#28965),(#28966,
#28967),(#28968,#28969),(#28970,#28971),(#28972,#28973),(#28974,#28975),
(#28976,#28977),(#28978,#28979),(#28980,#28981),(#28982,#28983),(#28984,
#28985),(#28986,#28987),(#28988,#28989),(#28990,#28991),(#28992,#28993),
(#28994,#28995),(#28996,#28997),(#28998,#28999),(#29000,#29001),(#29002,
#29003),(#29004,#29005),(#29006,#29007),(#29008,#29009),(#29010,#29011),
(#29012,#29013),(#29014,#29015),(#29016,#29017),(#29018,#29019),(#29020,
#29021),(#29022,#29023),(#29024,#29025),(#29026,#29027),(#29028,#29029),
(#29030,#29031),(#29032,#29033),(#29034,#29035),(#29036,#29037),(#29038,
#29039),(#29040,#29041),(#29042,#29043),(#29044,#29045),(#29046,#29047),
(#29048,#29049),(#29050,#29051),(#29052,#29053),(#29054,#29055),(#29056,
#29057),(#29058,#29059),(#29060,#29061),(#29062,#29063),(#29064,#29065),
(#29066,#29067),(#29068,#29069),(#29070,#29071),(#29072,#29073),(#29074,
#29075),(#29076,#29077),(#29078,#29079),(#29080,#29081),(#29082,#29083),
(#29084,#29085),(#29086,#29087),(#29088,#29089),(#29090,#29091),(#29092,
#29093),(#29094,#29095),(#29096,#29097),(#29098,#29099)),.UNSPECIFIED.,
 .F.,.F.,.F.)
B_SPLINE_SURFACE_WITH_KNOTS((6,1,1,1,1,1,1,1,1,1,1,1,1,1,1,1,1,1,1,1,1,
1,1,1,1,1,1,1,1,1,1,1,1,1,1,1,1,1,1,1,1,1,1,1,1,1,1,1,1,1,1,1,1,1,1,1,1,
1,1,1,1,1,1,1,1,6),(2,2),(-1.,-0.984615384615383,-0.969230769230768,-0.953846153846152,
-0.938461538461537,-0.923076923076922,-0.907692307692306,-0.892307692307691,
-0.876923076923076,-0.86153846153846,-0.846153846153845,-0.83076923076923,
-0.815384615384614,-0.799999999999999,-0.784615384615384,-0.769230769230768,
-0.753846153846153,-0.738461538461538,-0.723076923076922,-0.707692307692307,
-0.692307692307692,-0.676923076923076,-0.661538461538461,-0.646153846153846,
-0.63076923076923,-0.615384615384615,-0.6,-0.584615384615384,-0.569230769230769,
-0.553846153846154,-0.538461538461538,-0.523076923076923,-0.507692307692308,
-0.492307692307692,-0.476923076923077,-0.461538461538462,-0.446153846153846,
-0.430769230769231,-0.415384615384615,-0.4,-0.384615384615385,-0.369230769230769,
-0.353846153846154,-0.338461538461538,-0.323076923076923,-0.307692307692308,
-0.292307692307692,-0.276923076923077,-0.261538461538462,-0.246153846153846,
-0.230769230769231,-0.215384615384615,-0.2,-0.184615384615385,-0.169230769230769,
-0.153846153846154,-0.138461538461538,-0.123076923076923,-0.107692307692308,
-0.0923076923076923,-0.0769230769230769,-0.0615384615384615,-0.0461538461538462,
-0.0307692307692308,-0.0153846153846154,0.),(-1.,1.),.UNSPECIFIED.)
GEOMETRIC_REPRESENTATION_ITEM()
RATIONAL_B_SPLINE_SURFACE(((1.,1.),(1.,1.),(1.,1.),(1.,1.),(1.,1.),(1.,
1.),(1.,1.),(1.,1.),(1.,1.),(1.,1.),(1.,1.),(1.,1.),(1.,1.),(1.,1.),(1.,
1.),(1.,1.),(1.,1.),(1.,1.),(1.,1.),(1.,1.),(1.,1.),(1.,1.),(1.,1.),(1.,
1.),(1.,1.),(1.,1.),(1.,1.),(1.,1.),(1.,1.),(1.,1.),(1.,1.),(1.,1.),(1.,
1.),(1.,1.),(1.,1.),(1.,1.),(1.,1.),(1.,1.),(1.,1.),(1.,1.),(1.,1.),(1.,
1.),(1.,1.),(1.,1.),(1.,1.),(1.,1.),(1.,1.),(1.,1.),(1.,1.),(1.,1.),(1.,
1.),(1.,1.),(1.,1.),(1.,1.),(1.,1.),(1.,1.),(1.,1.),(1.,1.),(1.,1.),(1.,
1.),(1.,1.),(1.,1.),(1.,1.),(1.,1.),(1.,1.),(1.,1.),(1.,1.),(1.,1.),(1.,
1.),(1.,1.)))
REPRESENTATION_ITEM('')
SURFACE()
);
#36=(
BOUNDED_SURFACE()
B_SPLINE_SURFACE(5,1,((#29176,#29177),(#29178,#29179),(#29180,#29181),(#29182,
#29183),(#29184,#29185),(#29186,#29187),(#29188,#29189),(#29190,#29191),
(#29192,#29193),(#29194,#29195),(#29196,#29197),(#29198,#29199),(#29200,
#29201),(#29202,#29203),(#29204,#29205),(#29206,#29207),(#29208,#29209),
(#29210,#29211),(#29212,#29213),(#29214,#29215),(#29216,#29217),(#29218,
#29219),(#29220,#29221),(#29222,#29223),(#29224,#29225),(#29226,#29227),
(#29228,#29229),(#29230,#29231),(#29232,#29233),(#29234,#29235),(#29236,
#29237),(#29238,#29239),(#29240,#29241),(#29242,#29243),(#29244,#29245),
(#29246,#29247),(#29248,#29249),(#29250,#29251),(#29252,#29253),(#29254,
#29255),(#29256,#29257),(#29258,#29259),(#29260,#29261),(#29262,#29263),
(#29264,#29265),(#29266,#29267),(#29268,#29269),(#29270,#29271),(#29272,
#29273),(#29274,#29275),(#29276,#29277),(#29278,#29279),(#29280,#29281),
(#29282,#29283),(#29284,#29285),(#29286,#29287),(#29288,#29289),(#29290,
#29291),(#29292,#29293),(#29294,#29295),(#29296,#29297),(#29298,#29299),
(#29300,#29301),(#29302,#29303),(#29304,#29305),(#29306,#29307),(#29308,
#29309),(#29310,#29311),(#29312,#29313),(#29314,#29315)),.UNSPECIFIED.,
 .F.,.F.,.F.)
B_SPLINE_SURFACE_WITH_KNOTS((6,1,1,1,1,1,1,1,1,1,1,1,1,1,1,1,1,1,1,1,1,
1,1,1,1,1,1,1,1,1,1,1,1,1,1,1,1,1,1,1,1,1,1,1,1,1,1,1,1,1,1,1,1,1,1,1,1,
1,1,1,1,1,1,1,1,6),(2,2),(-1.,-0.984615384615383,-0.969230769230768,-0.953846153846152,
-0.938461538461537,-0.923076923076922,-0.907692307692306,-0.892307692307691,
-0.876923076923076,-0.86153846153846,-0.846153846153845,-0.83076923076923,
-0.815384615384614,-0.799999999999999,-0.784615384615384,-0.769230769230768,
-0.753846153846153,-0.738461538461538,-0.723076923076922,-0.707692307692307,
-0.692307692307692,-0.676923076923076,-0.661538461538461,-0.646153846153846,
-0.63076923076923,-0.615384615384615,-0.6,-0.584615384615384,-0.569230769230769,
-0.553846153846154,-0.538461538461538,-0.523076923076923,-0.507692307692308,
-0.492307692307692,-0.476923076923077,-0.461538461538462,-0.446153846153846,
-0.430769230769231,-0.415384615384615,-0.4,-0.384615384615385,-0.369230769230769,
-0.353846153846154,-0.338461538461538,-0.323076923076923,-0.307692307692308,
-0.292307692307692,-0.276923076923077,-0.261538461538462,-0.246153846153846,
-0.230769230769231,-0.215384615384615,-0.2,-0.184615384615385,-0.169230769230769,
-0.153846153846154,-0.138461538461538,-0.123076923076923,-0.107692307692308,
-0.0923076923076923,-0.0769230769230769,-0.0615384615384615,-0.0461538461538462,
-0.0307692307692308,-0.0153846153846154,0.),(-1.,1.),.UNSPECIFIED.)
GEOMETRIC_REPRESENTATION_ITEM()
RATIONAL_B_SPLINE_SURFACE(((1.,1.),(1.,1.),(1.,1.),(1.,1.),(1.,1.),(1.,
1.),(1.,1.),(1.,1.),(1.,1.),(1.,1.),(1.,1.),(1.,1.),(1.,1.),(1.,1.),(1.,
1.),(1.,1.),(1.,1.),(1.,1.),(1.,1.),(1.,1.),(1.,1.),(1.,1.),(1.,1.),(1.,
1.),(1.,1.),(1.,1.),(1.,1.),(1.,1.),(1.,1.),(1.,1.),(1.,1.),(1.,1.),(1.,
1.),(1.,1.),(1.,1.),(1.,1.),(1.,1.),(1.,1.),(1.,1.),(1.,1.),(1.,1.),(1.,
1.),(1.,1.),(1.,1.),(1.,1.),(1.,1.),(1.,1.),(1.,1.),(1.,1.),(1.,1.),(1.,
1.),(1.,1.),(1.,1.),(1.,1.),(1.,1.),(1.,1.),(1.,1.),(1.,1.),(1.,1.),(1.,
1.),(1.,1.),(1.,1.),(1.,1.),(1.,1.),(1.,1.),(1.,1.),(1.,1.),(1.,1.),(1.,
1.),(1.,1.)))
REPRESENTATION_ITEM('')
SURFACE()
);
#37=(
BOUNDED_SURFACE()
B_SPLINE_SURFACE(5,1,((#29392,#29393),(#29394,#29395),(#29396,#29397),(#29398,
#29399),(#29400,#29401),(#29402,#29403),(#29404,#29405),(#29406,#29407),
(#29408,#29409),(#29410,#29411),(#29412,#29413),(#29414,#29415),(#29416,
#29417),(#29418,#29419),(#29420,#29421),(#29422,#29423),(#29424,#29425),
(#29426,#29427),(#29428,#29429),(#29430,#29431),(#29432,#29433),(#29434,
#29435),(#29436,#29437),(#29438,#29439),(#29440,#29441),(#29442,#29443),
(#29444,#29445),(#29446,#29447),(#29448,#29449),(#29450,#29451),(#29452,
#29453),(#29454,#29455),(#29456,#29457),(#29458,#29459),(#29460,#29461),
(#29462,#29463),(#29464,#29465),(#29466,#29467),(#29468,#29469),(#29470,
#29471),(#29472,#29473),(#29474,#29475),(#29476,#29477),(#29478,#29479),
(#29480,#29481),(#29482,#29483),(#29484,#29485),(#29486,#29487),(#29488,
#29489),(#29490,#29491),(#29492,#29493),(#29494,#29495),(#29496,#29497),
(#29498,#29499),(#29500,#29501),(#29502,#29503),(#29504,#29505),(#29506,
#29507),(#29508,#29509),(#29510,#29511),(#29512,#29513),(#29514,#29515),
(#29516,#29517),(#29518,#29519),(#29520,#29521),(#29522,#29523),(#29524,
#29525),(#29526,#29527),(#29528,#29529),(#29530,#29531)),.UNSPECIFIED.,
 .F.,.F.,.F.)
B_SPLINE_SURFACE_WITH_KNOTS((6,1,1,1,1,1,1,1,1,1,1,1,1,1,1,1,1,1,1,1,1,
1,1,1,1,1,1,1,1,1,1,1,1,1,1,1,1,1,1,1,1,1,1,1,1,1,1,1,1,1,1,1,1,1,1,1,1,
1,1,1,1,1,1,1,1,6),(2,2),(-1.,-0.984615384615383,-0.969230769230768,-0.953846153846152,
-0.938461538461537,-0.923076923076922,-0.907692307692306,-0.892307692307691,
-0.876923076923076,-0.86153846153846,-0.846153846153845,-0.83076923076923,
-0.815384615384614,-0.799999999999999,-0.784615384615384,-0.769230769230768,
-0.753846153846153,-0.738461538461538,-0.723076923076922,-0.707692307692307,
-0.692307692307692,-0.676923076923076,-0.661538461538461,-0.646153846153846,
-0.63076923076923,-0.615384615384615,-0.6,-0.584615384615384,-0.569230769230769,
-0.553846153846154,-0.538461538461538,-0.523076923076923,-0.507692307692308,
-0.492307692307692,-0.476923076923077,-0.461538461538462,-0.446153846153846,
-0.430769230769231,-0.415384615384615,-0.4,-0.384615384615385,-0.369230769230769,
-0.353846153846154,-0.338461538461538,-0.323076923076923,-0.307692307692308,
-0.292307692307692,-0.276923076923077,-0.261538461538462,-0.246153846153846,
-0.230769230769231,-0.215384615384615,-0.2,-0.184615384615385,-0.169230769230769,
-0.153846153846154,-0.138461538461538,-0.123076923076923,-0.107692307692308,
-0.0923076923076923,-0.0769230769230769,-0.0615384615384615,-0.0461538461538462,
-0.0307692307692308,-0.0153846153846154,0.),(-1.,1.),.UNSPECIFIED.)
GEOMETRIC_REPRESENTATION_ITEM()
RATIONAL_B_SPLINE_SURFACE(((1.,1.),(1.,1.),(1.,1.),(1.,1.),(1.,1.),(1.,
1.),(1.,1.),(1.,1.),(1.,1.),(1.,1.),(1.,1.),(1.,1.),(1.,1.),(1.,1.),(1.,
1.),(1.,1.),(1.,1.),(1.,1.),(1.,1.),(1.,1.),(1.,1.),(1.,1.),(1.,1.),(1.,
1.),(1.,1.),(1.,1.),(1.,1.),(1.,1.),(1.,1.),(1.,1.),(1.,1.),(1.,1.),(1.,
1.),(1.,1.),(1.,1.),(1.,1.),(1.,1.),(1.,1.),(1.,1.),(1.,1.),(1.,1.),(1.,
1.),(1.,1.),(1.,1.),(1.,1.),(1.,1.),(1.,1.),(1.,1.),(1.,1.),(1.,1.),(1.,
1.),(1.,1.),(1.,1.),(1.,1.),(1.,1.),(1.,1.),(1.,1.),(1.,1.),(1.,1.),(1.,
1.),(1.,1.),(1.,1.),(1.,1.),(1.,1.),(1.,1.),(1.,1.),(1.,1.),(1.,1.),(1.,
1.),(1.,1.)))
REPRESENTATION_ITEM('')
SURFACE()
);
#38=(
BOUNDED_SURFACE()
B_SPLINE_SURFACE(5,1,((#29608,#29609),(#29610,#29611),(#29612,#29613),(#29614,
#29615),(#29616,#29617),(#29618,#29619),(#29620,#29621),(#29622,#29623),
(#29624,#29625),(#29626,#29627),(#29628,#29629),(#29630,#29631),(#29632,
#29633),(#29634,#29635),(#29636,#29637),(#29638,#29639),(#29640,#29641),
(#29642,#29643),(#29644,#29645),(#29646,#29647),(#29648,#29649),(#29650,
#29651),(#29652,#29653),(#29654,#29655),(#29656,#29657),(#29658,#29659),
(#29660,#29661),(#29662,#29663),(#29664,#29665),(#29666,#29667),(#29668,
#29669),(#29670,#29671),(#29672,#29673),(#29674,#29675),(#29676,#29677),
(#29678,#29679),(#29680,#29681),(#29682,#29683),(#29684,#29685),(#29686,
#29687),(#29688,#29689),(#29690,#29691),(#29692,#29693),(#29694,#29695),
(#29696,#29697),(#29698,#29699),(#29700,#29701),(#29702,#29703),(#29704,
#29705),(#29706,#29707),(#29708,#29709),(#29710,#29711),(#29712,#29713),
(#29714,#29715),(#29716,#29717),(#29718,#29719),(#29720,#29721),(#29722,
#29723),(#29724,#29725),(#29726,#29727),(#29728,#29729),(#29730,#29731),
(#29732,#29733),(#29734,#29735),(#29736,#29737),(#29738,#29739),(#29740,
#29741),(#29742,#29743),(#29744,#29745),(#29746,#29747)),.UNSPECIFIED.,
 .F.,.F.,.F.)
B_SPLINE_SURFACE_WITH_KNOTS((6,1,1,1,1,1,1,1,1,1,1,1,1,1,1,1,1,1,1,1,1,
1,1,1,1,1,1,1,1,1,1,1,1,1,1,1,1,1,1,1,1,1,1,1,1,1,1,1,1,1,1,1,1,1,1,1,1,
1,1,1,1,1,1,1,1,6),(2,2),(-1.,-0.984615384615383,-0.969230769230768,-0.953846153846152,
-0.938461538461537,-0.923076923076922,-0.907692307692306,-0.892307692307691,
-0.876923076923076,-0.86153846153846,-0.846153846153845,-0.83076923076923,
-0.815384615384614,-0.799999999999999,-0.784615384615384,-0.769230769230768,
-0.753846153846153,-0.738461538461538,-0.723076923076922,-0.707692307692307,
-0.692307692307692,-0.676923076923076,-0.661538461538461,-0.646153846153846,
-0.63076923076923,-0.615384615384615,-0.6,-0.584615384615384,-0.569230769230769,
-0.553846153846154,-0.538461538461538,-0.523076923076923,-0.507692307692308,
-0.492307692307692,-0.476923076923077,-0.461538461538462,-0.446153846153846,
-0.430769230769231,-0.415384615384615,-0.4,-0.384615384615385,-0.369230769230769,
-0.353846153846154,-0.338461538461538,-0.323076923076923,-0.307692307692308,
-0.292307692307692,-0.276923076923077,-0.261538461538462,-0.246153846153846,
-0.230769230769231,-0.215384615384615,-0.2,-0.184615384615385,-0.169230769230769,
-0.153846153846154,-0.138461538461538,-0.123076923076923,-0.107692307692308,
-0.0923076923076923,-0.0769230769230769,-0.0615384615384615,-0.0461538461538462,
-0.0307692307692308,-0.0153846153846154,0.),(-1.,1.),.UNSPECIFIED.)
GEOMETRIC_REPRESENTATION_ITEM()
RATIONAL_B_SPLINE_SURFACE(((1.,1.),(1.,1.),(1.,1.),(1.,1.),(1.,1.),(1.,
1.),(1.,1.),(1.,1.),(1.,1.),(1.,1.),(1.,1.),(1.,1.),(1.,1.),(1.,1.),(1.,
1.),(1.,1.),(1.,1.),(1.,1.),(1.,1.),(1.,1.),(1.,1.),(1.,1.),(1.,1.),(1.,
1.),(1.,1.),(1.,1.),(1.,1.),(1.,1.),(1.,1.),(1.,1.),(1.,1.),(1.,1.),(1.,
1.),(1.,1.),(1.,1.),(1.,1.),(1.,1.),(1.,1.),(1.,1.),(1.,1.),(1.,1.),(1.,
1.),(1.,1.),(1.,1.),(1.,1.),(1.,1.),(1.,1.),(1.,1.),(1.,1.),(1.,1.),(1.,
1.),(1.,1.),(1.,1.),(1.,1.),(1.,1.),(1.,1.),(1.,1.),(1.,1.),(1.,1.),(1.,
1.),(1.,1.),(1.,1.),(1.,1.),(1.,1.),(1.,1.),(1.,1.),(1.,1.),(1.,1.),(1.,
1.),(1.,1.)))
REPRESENTATION_ITEM('')
SURFACE()
);
#39=(
BOUNDED_SURFACE()
B_SPLINE_SURFACE(5,1,((#29824,#29825),(#29826,#29827),(#29828,#29829),(#29830,
#29831),(#29832,#29833),(#29834,#29835),(#29836,#29837),(#29838,#29839),
(#29840,#29841),(#29842,#29843),(#29844,#29845),(#29846,#29847),(#29848,
#29849),(#29850,#29851),(#29852,#29853),(#29854,#29855),(#29856,#29857),
(#29858,#29859),(#29860,#29861),(#29862,#29863),(#29864,#29865),(#29866,
#29867),(#29868,#29869),(#29870,#29871),(#29872,#29873),(#29874,#29875),
(#29876,#29877),(#29878,#29879),(#29880,#29881),(#29882,#29883),(#29884,
#29885),(#29886,#29887),(#29888,#29889),(#29890,#29891),(#29892,#29893),
(#29894,#29895),(#29896,#29897),(#29898,#29899),(#29900,#29901),(#29902,
#29903),(#29904,#29905),(#29906,#29907),(#29908,#29909),(#29910,#29911),
(#29912,#29913),(#29914,#29915),(#29916,#29917),(#29918,#29919),(#29920,
#29921),(#29922,#29923),(#29924,#29925),(#29926,#29927),(#29928,#29929),
(#29930,#29931),(#29932,#29933),(#29934,#29935),(#29936,#29937),(#29938,
#29939),(#29940,#29941),(#29942,#29943),(#29944,#29945),(#29946,#29947),
(#29948,#29949),(#29950,#29951),(#29952,#29953),(#29954,#29955),(#29956,
#29957),(#29958,#29959),(#29960,#29961),(#29962,#29963)),.UNSPECIFIED.,
 .F.,.F.,.F.)
B_SPLINE_SURFACE_WITH_KNOTS((6,1,1,1,1,1,1,1,1,1,1,1,1,1,1,1,1,1,1,1,1,
1,1,1,1,1,1,1,1,1,1,1,1,1,1,1,1,1,1,1,1,1,1,1,1,1,1,1,1,1,1,1,1,1,1,1,1,
1,1,1,1,1,1,1,1,6),(2,2),(-1.,-0.984615384615383,-0.969230769230768,-0.953846153846152,
-0.938461538461537,-0.923076923076922,-0.907692307692306,-0.892307692307691,
-0.876923076923076,-0.86153846153846,-0.846153846153845,-0.83076923076923,
-0.815384615384614,-0.799999999999999,-0.784615384615384,-0.769230769230768,
-0.753846153846153,-0.738461538461538,-0.723076923076922,-0.707692307692307,
-0.692307692307692,-0.676923076923076,-0.661538461538461,-0.646153846153846,
-0.63076923076923,-0.615384615384615,-0.6,-0.584615384615384,-0.569230769230769,
-0.553846153846154,-0.538461538461538,-0.523076923076923,-0.507692307692308,
-0.492307692307692,-0.476923076923077,-0.461538461538462,-0.446153846153846,
-0.430769230769231,-0.415384615384615,-0.4,-0.384615384615385,-0.369230769230769,
-0.353846153846154,-0.338461538461538,-0.323076923076923,-0.307692307692308,
-0.292307692307692,-0.276923076923077,-0.261538461538462,-0.246153846153846,
-0.230769230769231,-0.215384615384615,-0.2,-0.184615384615385,-0.169230769230769,
-0.153846153846154,-0.138461538461538,-0.123076923076923,-0.107692307692308,
-0.0923076923076923,-0.0769230769230769,-0.0615384615384615,-0.0461538461538462,
-0.0307692307692308,-0.0153846153846154,0.),(-1.,1.),.UNSPECIFIED.)
GEOMETRIC_REPRESENTATION_ITEM()
RATIONAL_B_SPLINE_SURFACE(((1.,1.),(1.,1.),(1.,1.),(1.,1.),(1.,1.),(1.,
1.),(1.,1.),(1.,1.),(1.,1.),(1.,1.),(1.,1.),(1.,1.),(1.,1.),(1.,1.),(1.,
1.),(1.,1.),(1.,1.),(1.,1.),(1.,1.),(1.,1.),(1.,1.),(1.,1.),(1.,1.),(1.,
1.),(1.,1.),(1.,1.),(1.,1.),(1.,1.),(1.,1.),(1.,1.),(1.,1.),(1.,1.),(1.,
1.),(1.,1.),(1.,1.),(1.,1.),(1.,1.),(1.,1.),(1.,1.),(1.,1.),(1.,1.),(1.,
1.),(1.,1.),(1.,1.),(1.,1.),(1.,1.),(1.,1.),(1.,1.),(1.,1.),(1.,1.),(1.,
1.),(1.,1.),(1.,1.),(1.,1.),(1.,1.),(1.,1.),(1.,1.),(1.,1.),(1.,1.),(1.,
1.),(1.,1.),(1.,1.),(1.,1.),(1.,1.),(1.,1.),(1.,1.),(1.,1.),(1.,1.),(1.,
1.),(1.,1.)))
REPRESENTATION_ITEM('')
SURFACE()
);
#40=(
BOUNDED_SURFACE()
B_SPLINE_SURFACE(5,1,((#30040,#30041),(#30042,#30043),(#30044,#30045),(#30046,
#30047),(#30048,#30049),(#30050,#30051),(#30052,#30053),(#30054,#30055),
(#30056,#30057),(#30058,#30059),(#30060,#30061),(#30062,#30063),(#30064,
#30065),(#30066,#30067),(#30068,#30069),(#30070,#30071),(#30072,#30073),
(#30074,#30075),(#30076,#30077),(#30078,#30079),(#30080,#30081),(#30082,
#30083),(#30084,#30085),(#30086,#30087),(#30088,#30089),(#30090,#30091),
(#30092,#30093),(#30094,#30095),(#30096,#30097),(#30098,#30099),(#30100,
#30101),(#30102,#30103),(#30104,#30105),(#30106,#30107),(#30108,#30109),
(#30110,#30111),(#30112,#30113),(#30114,#30115),(#30116,#30117),(#30118,
#30119),(#30120,#30121),(#30122,#30123),(#30124,#30125),(#30126,#30127),
(#30128,#30129),(#30130,#30131),(#30132,#30133),(#30134,#30135),(#30136,
#30137),(#30138,#30139),(#30140,#30141),(#30142,#30143),(#30144,#30145),
(#30146,#30147),(#30148,#30149),(#30150,#30151),(#30152,#30153),(#30154,
#30155),(#30156,#30157),(#30158,#30159),(#30160,#30161),(#30162,#30163),
(#30164,#30165),(#30166,#30167),(#30168,#30169),(#30170,#30171),(#30172,
#30173),(#30174,#30175),(#30176,#30177),(#30178,#30179)),.UNSPECIFIED.,
 .F.,.F.,.F.)
B_SPLINE_SURFACE_WITH_KNOTS((6,1,1,1,1,1,1,1,1,1,1,1,1,1,1,1,1,1,1,1,1,
1,1,1,1,1,1,1,1,1,1,1,1,1,1,1,1,1,1,1,1,1,1,1,1,1,1,1,1,1,1,1,1,1,1,1,1,
1,1,1,1,1,1,1,1,6),(2,2),(-1.,-0.984615384615383,-0.969230769230768,-0.953846153846152,
-0.938461538461537,-0.923076923076922,-0.907692307692306,-0.892307692307691,
-0.876923076923076,-0.86153846153846,-0.846153846153845,-0.83076923076923,
-0.815384615384614,-0.799999999999999,-0.784615384615384,-0.769230769230768,
-0.753846153846153,-0.738461538461538,-0.723076923076922,-0.707692307692307,
-0.692307692307692,-0.676923076923076,-0.661538461538461,-0.646153846153846,
-0.63076923076923,-0.615384615384615,-0.6,-0.584615384615384,-0.569230769230769,
-0.553846153846154,-0.538461538461538,-0.523076923076923,-0.507692307692308,
-0.492307692307692,-0.476923076923077,-0.461538461538462,-0.446153846153846,
-0.430769230769231,-0.415384615384615,-0.4,-0.384615384615385,-0.369230769230769,
-0.353846153846154,-0.338461538461538,-0.323076923076923,-0.307692307692308,
-0.292307692307692,-0.276923076923077,-0.261538461538462,-0.246153846153846,
-0.230769230769231,-0.215384615384615,-0.2,-0.184615384615385,-0.169230769230769,
-0.153846153846154,-0.138461538461538,-0.123076923076923,-0.107692307692308,
-0.0923076923076923,-0.0769230769230769,-0.0615384615384615,-0.0461538461538462,
-0.0307692307692308,-0.0153846153846154,0.),(-1.,1.),.UNSPECIFIED.)
GEOMETRIC_REPRESENTATION_ITEM()
RATIONAL_B_SPLINE_SURFACE(((1.,1.),(1.,1.),(1.,1.),(1.,1.),(1.,1.),(1.,
1.),(1.,1.),(1.,1.),(1.,1.),(1.,1.),(1.,1.),(1.,1.),(1.,1.),(1.,1.),(1.,
1.),(1.,1.),(1.,1.),(1.,1.),(1.,1.),(1.,1.),(1.,1.),(1.,1.),(1.,1.),(1.,
1.),(1.,1.),(1.,1.),(1.,1.),(1.,1.),(1.,1.),(1.,1.),(1.,1.),(1.,1.),(1.,
1.),(1.,1.),(1.,1.),(1.,1.),(1.,1.),(1.,1.),(1.,1.),(1.,1.),(1.,1.),(1.,
1.),(1.,1.),(1.,1.),(1.,1.),(1.,1.),(1.,1.),(1.,1.),(1.,1.),(1.,1.),(1.,
1.),(1.,1.),(1.,1.),(1.,1.),(1.,1.),(1.,1.),(1.,1.),(1.,1.),(1.,1.),(1.,
1.),(1.,1.),(1.,1.),(1.,1.),(1.,1.),(1.,1.),(1.,1.),(1.,1.),(1.,1.),(1.,
1.),(1.,1.)))
REPRESENTATION_ITEM('')
SURFACE()
);
#41=(
BOUNDED_SURFACE()
B_SPLINE_SURFACE(5,1,((#30256,#30257),(#30258,#30259),(#30260,#30261),(#30262,
#30263),(#30264,#30265),(#30266,#30267),(#30268,#30269),(#30270,#30271),
(#30272,#30273),(#30274,#30275),(#30276,#30277),(#30278,#30279),(#30280,
#30281),(#30282,#30283),(#30284,#30285),(#30286,#30287),(#30288,#30289),
(#30290,#30291),(#30292,#30293),(#30294,#30295),(#30296,#30297),(#30298,
#30299),(#30300,#30301),(#30302,#30303),(#30304,#30305),(#30306,#30307),
(#30308,#30309),(#30310,#30311),(#30312,#30313),(#30314,#30315),(#30316,
#30317),(#30318,#30319),(#30320,#30321),(#30322,#30323),(#30324,#30325),
(#30326,#30327),(#30328,#30329),(#30330,#30331),(#30332,#30333),(#30334,
#30335),(#30336,#30337),(#30338,#30339),(#30340,#30341),(#30342,#30343),
(#30344,#30345),(#30346,#30347),(#30348,#30349),(#30350,#30351),(#30352,
#30353),(#30354,#30355),(#30356,#30357),(#30358,#30359),(#30360,#30361),
(#30362,#30363),(#30364,#30365),(#30366,#30367),(#30368,#30369),(#30370,
#30371),(#30372,#30373),(#30374,#30375),(#30376,#30377),(#30378,#30379),
(#30380,#30381),(#30382,#30383),(#30384,#30385),(#30386,#30387),(#30388,
#30389),(#30390,#30391),(#30392,#30393),(#30394,#30395)),.UNSPECIFIED.,
 .F.,.F.,.F.)
B_SPLINE_SURFACE_WITH_KNOTS((6,1,1,1,1,1,1,1,1,1,1,1,1,1,1,1,1,1,1,1,1,
1,1,1,1,1,1,1,1,1,1,1,1,1,1,1,1,1,1,1,1,1,1,1,1,1,1,1,1,1,1,1,1,1,1,1,1,
1,1,1,1,1,1,1,1,6),(2,2),(-1.,-0.984615384615383,-0.969230769230768,-0.953846153846152,
-0.938461538461537,-0.923076923076922,-0.907692307692306,-0.892307692307691,
-0.876923076923076,-0.86153846153846,-0.846153846153845,-0.83076923076923,
-0.815384615384614,-0.799999999999999,-0.784615384615384,-0.769230769230768,
-0.753846153846153,-0.738461538461538,-0.723076923076922,-0.707692307692307,
-0.692307692307692,-0.676923076923076,-0.661538461538461,-0.646153846153846,
-0.63076923076923,-0.615384615384615,-0.6,-0.584615384615384,-0.569230769230769,
-0.553846153846154,-0.538461538461538,-0.523076923076923,-0.507692307692308,
-0.492307692307692,-0.476923076923077,-0.461538461538462,-0.446153846153846,
-0.430769230769231,-0.415384615384615,-0.4,-0.384615384615385,-0.369230769230769,
-0.353846153846154,-0.338461538461538,-0.323076923076923,-0.307692307692308,
-0.292307692307692,-0.276923076923077,-0.261538461538462,-0.246153846153846,
-0.230769230769231,-0.215384615384615,-0.2,-0.184615384615385,-0.169230769230769,
-0.153846153846154,-0.138461538461538,-0.123076923076923,-0.107692307692308,
-0.0923076923076923,-0.0769230769230769,-0.0615384615384615,-0.0461538461538462,
-0.0307692307692308,-0.0153846153846154,0.),(-1.,1.),.UNSPECIFIED.)
GEOMETRIC_REPRESENTATION_ITEM()
RATIONAL_B_SPLINE_SURFACE(((1.,1.),(1.,1.),(1.,1.),(1.,1.),(1.,1.),(1.,
1.),(1.,1.),(1.,1.),(1.,1.),(1.,1.),(1.,1.),(1.,1.),(1.,1.),(1.,1.),(1.,
1.),(1.,1.),(1.,1.),(1.,1.),(1.,1.),(1.,1.),(1.,1.),(1.,1.),(1.,1.),(1.,
1.),(1.,1.),(1.,1.),(1.,1.),(1.,1.),(1.,1.),(1.,1.),(1.,1.),(1.,1.),(1.,
1.),(1.,1.),(1.,1.),(1.,1.),(1.,1.),(1.,1.),(1.,1.),(1.,1.),(1.,1.),(1.,
1.),(1.,1.),(1.,1.),(1.,1.),(1.,1.),(1.,1.),(1.,1.),(1.,1.),(1.,1.),(1.,
1.),(1.,1.),(1.,1.),(1.,1.),(1.,1.),(1.,1.),(1.,1.),(1.,1.),(1.,1.),(1.,
1.),(1.,1.),(1.,1.),(1.,1.),(1.,1.),(1.,1.),(1.,1.),(1.,1.),(1.,1.),(1.,
1.),(1.,1.)))
REPRESENTATION_ITEM('')
SURFACE()
);
#42=(
BOUNDED_SURFACE()
B_SPLINE_SURFACE(5,1,((#30472,#30473),(#30474,#30475),(#30476,#30477),(#30478,
#30479),(#30480,#30481),(#30482,#30483),(#30484,#30485),(#30486,#30487),
(#30488,#30489),(#30490,#30491),(#30492,#30493),(#30494,#30495),(#30496,
#30497),(#30498,#30499),(#30500,#30501),(#30502,#30503),(#30504,#30505),
(#30506,#30507),(#30508,#30509),(#30510,#30511),(#30512,#30513),(#30514,
#30515),(#30516,#30517),(#30518,#30519),(#30520,#30521),(#30522,#30523),
(#30524,#30525),(#30526,#30527),(#30528,#30529),(#30530,#30531),(#30532,
#30533),(#30534,#30535),(#30536,#30537),(#30538,#30539),(#30540,#30541),
(#30542,#30543),(#30544,#30545),(#30546,#30547),(#30548,#30549),(#30550,
#30551),(#30552,#30553),(#30554,#30555),(#30556,#30557),(#30558,#30559),
(#30560,#30561),(#30562,#30563),(#30564,#30565),(#30566,#30567),(#30568,
#30569),(#30570,#30571),(#30572,#30573),(#30574,#30575),(#30576,#30577),
(#30578,#30579),(#30580,#30581),(#30582,#30583),(#30584,#30585),(#30586,
#30587),(#30588,#30589),(#30590,#30591),(#30592,#30593),(#30594,#30595),
(#30596,#30597),(#30598,#30599),(#30600,#30601),(#30602,#30603),(#30604,
#30605),(#30606,#30607),(#30608,#30609),(#30610,#30611)),.UNSPECIFIED.,
 .F.,.F.,.F.)
B_SPLINE_SURFACE_WITH_KNOTS((6,1,1,1,1,1,1,1,1,1,1,1,1,1,1,1,1,1,1,1,1,
1,1,1,1,1,1,1,1,1,1,1,1,1,1,1,1,1,1,1,1,1,1,1,1,1,1,1,1,1,1,1,1,1,1,1,1,
1,1,1,1,1,1,1,1,6),(2,2),(-1.,-0.984615384615383,-0.969230769230768,-0.953846153846152,
-0.938461538461537,-0.923076923076922,-0.907692307692306,-0.892307692307691,
-0.876923076923076,-0.86153846153846,-0.846153846153845,-0.83076923076923,
-0.815384615384614,-0.799999999999999,-0.784615384615384,-0.769230769230768,
-0.753846153846153,-0.738461538461538,-0.723076923076922,-0.707692307692307,
-0.692307692307692,-0.676923076923076,-0.661538461538461,-0.646153846153846,
-0.63076923076923,-0.615384615384615,-0.6,-0.584615384615384,-0.569230769230769,
-0.553846153846154,-0.538461538461538,-0.523076923076923,-0.507692307692308,
-0.492307692307692,-0.476923076923077,-0.461538461538462,-0.446153846153846,
-0.430769230769231,-0.415384615384615,-0.4,-0.384615384615385,-0.369230769230769,
-0.353846153846154,-0.338461538461538,-0.323076923076923,-0.307692307692308,
-0.292307692307692,-0.276923076923077,-0.261538461538462,-0.246153846153846,
-0.230769230769231,-0.215384615384615,-0.2,-0.184615384615385,-0.169230769230769,
-0.153846153846154,-0.138461538461538,-0.123076923076923,-0.107692307692308,
-0.0923076923076923,-0.0769230769230769,-0.0615384615384615,-0.0461538461538462,
-0.0307692307692308,-0.0153846153846154,0.),(-1.,1.),.UNSPECIFIED.)
GEOMETRIC_REPRESENTATION_ITEM()
RATIONAL_B_SPLINE_SURFACE(((1.,1.),(1.,1.),(1.,1.),(1.,1.),(1.,1.),(1.,
1.),(1.,1.),(1.,1.),(1.,1.),(1.,1.),(1.,1.),(1.,1.),(1.,1.),(1.,1.),(1.,
1.),(1.,1.),(1.,1.),(1.,1.),(1.,1.),(1.,1.),(1.,1.),(1.,1.),(1.,1.),(1.,
1.),(1.,1.),(1.,1.),(1.,1.),(1.,1.),(1.,1.),(1.,1.),(1.,1.),(1.,1.),(1.,
1.),(1.,1.),(1.,1.),(1.,1.),(1.,1.),(1.,1.),(1.,1.),(1.,1.),(1.,1.),(1.,
1.),(1.,1.),(1.,1.),(1.,1.),(1.,1.),(1.,1.),(1.,1.),(1.,1.),(1.,1.),(1.,
1.),(1.,1.),(1.,1.),(1.,1.),(1.,1.),(1.,1.),(1.,1.),(1.,1.),(1.,1.),(1.,
1.),(1.,1.),(1.,1.),(1.,1.),(1.,1.),(1.,1.),(1.,1.),(1.,1.),(1.,1.),(1.,
1.),(1.,1.)))
REPRESENTATION_ITEM('')
SURFACE()
);
#43=(
BOUNDED_SURFACE()
B_SPLINE_SURFACE(5,1,((#30688,#30689),(#30690,#30691),(#30692,#30693),(#30694,
#30695),(#30696,#30697),(#30698,#30699),(#30700,#30701),(#30702,#30703),
(#30704,#30705),(#30706,#30707),(#30708,#30709),(#30710,#30711),(#30712,
#30713),(#30714,#30715),(#30716,#30717),(#30718,#30719),(#30720,#30721),
(#30722,#30723),(#30724,#30725),(#30726,#30727),(#30728,#30729),(#30730,
#30731),(#30732,#30733),(#30734,#30735),(#30736,#30737),(#30738,#30739),
(#30740,#30741),(#30742,#30743),(#30744,#30745),(#30746,#30747),(#30748,
#30749),(#30750,#30751),(#30752,#30753),(#30754,#30755),(#30756,#30757),
(#30758,#30759),(#30760,#30761),(#30762,#30763),(#30764,#30765),(#30766,
#30767),(#30768,#30769),(#30770,#30771),(#30772,#30773),(#30774,#30775),
(#30776,#30777),(#30778,#30779),(#30780,#30781),(#30782,#30783),(#30784,
#30785),(#30786,#30787),(#30788,#30789),(#30790,#30791),(#30792,#30793),
(#30794,#30795),(#30796,#30797),(#30798,#30799),(#30800,#30801),(#30802,
#30803),(#30804,#30805),(#30806,#30807),(#30808,#30809),(#30810,#30811),
(#30812,#30813),(#30814,#30815),(#30816,#30817),(#30818,#30819),(#30820,
#30821),(#30822,#30823),(#30824,#30825),(#30826,#30827)),.UNSPECIFIED.,
 .F.,.F.,.F.)
B_SPLINE_SURFACE_WITH_KNOTS((6,1,1,1,1,1,1,1,1,1,1,1,1,1,1,1,1,1,1,1,1,
1,1,1,1,1,1,1,1,1,1,1,1,1,1,1,1,1,1,1,1,1,1,1,1,1,1,1,1,1,1,1,1,1,1,1,1,
1,1,1,1,1,1,1,1,6),(2,2),(-1.,-0.984615384615383,-0.969230769230768,-0.953846153846152,
-0.938461538461537,-0.923076923076922,-0.907692307692306,-0.892307692307691,
-0.876923076923076,-0.86153846153846,-0.846153846153845,-0.83076923076923,
-0.815384615384614,-0.799999999999999,-0.784615384615384,-0.769230769230768,
-0.753846153846153,-0.738461538461538,-0.723076923076922,-0.707692307692307,
-0.692307692307692,-0.676923076923076,-0.661538461538461,-0.646153846153846,
-0.63076923076923,-0.615384615384615,-0.6,-0.584615384615384,-0.569230769230769,
-0.553846153846154,-0.538461538461538,-0.523076923076923,-0.507692307692308,
-0.492307692307692,-0.476923076923077,-0.461538461538462,-0.446153846153846,
-0.430769230769231,-0.415384615384615,-0.4,-0.384615384615385,-0.369230769230769,
-0.353846153846154,-0.338461538461538,-0.323076923076923,-0.307692307692308,
-0.292307692307692,-0.276923076923077,-0.261538461538462,-0.246153846153846,
-0.230769230769231,-0.215384615384615,-0.2,-0.184615384615385,-0.169230769230769,
-0.153846153846154,-0.138461538461538,-0.123076923076923,-0.107692307692308,
-0.0923076923076923,-0.0769230769230769,-0.0615384615384615,-0.0461538461538462,
-0.0307692307692308,-0.0153846153846154,0.),(-1.,1.),.UNSPECIFIED.)
GEOMETRIC_REPRESENTATION_ITEM()
RATIONAL_B_SPLINE_SURFACE(((1.,1.),(1.,1.),(1.,1.),(1.,1.),(1.,1.),(1.,
1.),(1.,1.),(1.,1.),(1.,1.),(1.,1.),(1.,1.),(1.,1.),(1.,1.),(1.,1.),(1.,
1.),(1.,1.),(1.,1.),(1.,1.),(1.,1.),(1.,1.),(1.,1.),(1.,1.),(1.,1.),(1.,
1.),(1.,1.),(1.,1.),(1.,1.),(1.,1.),(1.,1.),(1.,1.),(1.,1.),(1.,1.),(1.,
1.),(1.,1.),(1.,1.),(1.,1.),(1.,1.),(1.,1.),(1.,1.),(1.,1.),(1.,1.),(1.,
1.),(1.,1.),(1.,1.),(1.,1.),(1.,1.),(1.,1.),(1.,1.),(1.,1.),(1.,1.),(1.,
1.),(1.,1.),(1.,1.),(1.,1.),(1.,1.),(1.,1.),(1.,1.),(1.,1.),(1.,1.),(1.,
1.),(1.,1.),(1.,1.),(1.,1.),(1.,1.),(1.,1.),(1.,1.),(1.,1.),(1.,1.),(1.,
1.),(1.,1.)))
REPRESENTATION_ITEM('')
SURFACE()
);
#44=(
BOUNDED_SURFACE()
B_SPLINE_SURFACE(5,1,((#30904,#30905),(#30906,#30907),(#30908,#30909),(#30910,
#30911),(#30912,#30913),(#30914,#30915),(#30916,#30917),(#30918,#30919),
(#30920,#30921),(#30922,#30923),(#30924,#30925),(#30926,#30927),(#30928,
#30929),(#30930,#30931),(#30932,#30933),(#30934,#30935),(#30936,#30937),
(#30938,#30939),(#30940,#30941),(#30942,#30943),(#30944,#30945),(#30946,
#30947),(#30948,#30949),(#30950,#30951),(#30952,#30953),(#30954,#30955),
(#30956,#30957),(#30958,#30959),(#30960,#30961),(#30962,#30963),(#30964,
#30965),(#30966,#30967),(#30968,#30969),(#30970,#30971),(#30972,#30973),
(#30974,#30975),(#30976,#30977),(#30978,#30979),(#30980,#30981),(#30982,
#30983),(#30984,#30985),(#30986,#30987),(#30988,#30989),(#30990,#30991),
(#30992,#30993),(#30994,#30995),(#30996,#30997),(#30998,#30999),(#31000,
#31001),(#31002,#31003),(#31004,#31005),(#31006,#31007),(#31008,#31009),
(#31010,#31011),(#31012,#31013),(#31014,#31015),(#31016,#31017),(#31018,
#31019),(#31020,#31021),(#31022,#31023),(#31024,#31025),(#31026,#31027),
(#31028,#31029),(#31030,#31031),(#31032,#31033),(#31034,#31035),(#31036,
#31037),(#31038,#31039),(#31040,#31041),(#31042,#31043)),.UNSPECIFIED.,
 .F.,.F.,.F.)
B_SPLINE_SURFACE_WITH_KNOTS((6,1,1,1,1,1,1,1,1,1,1,1,1,1,1,1,1,1,1,1,1,
1,1,1,1,1,1,1,1,1,1,1,1,1,1,1,1,1,1,1,1,1,1,1,1,1,1,1,1,1,1,1,1,1,1,1,1,
1,1,1,1,1,1,1,1,6),(2,2),(-1.,-0.984615384615383,-0.969230769230768,-0.953846153846152,
-0.938461538461537,-0.923076923076922,-0.907692307692306,-0.892307692307691,
-0.876923076923076,-0.86153846153846,-0.846153846153845,-0.83076923076923,
-0.815384615384614,-0.799999999999999,-0.784615384615384,-0.769230769230768,
-0.753846153846153,-0.738461538461538,-0.723076923076922,-0.707692307692307,
-0.692307692307692,-0.676923076923076,-0.661538461538461,-0.646153846153846,
-0.63076923076923,-0.615384615384615,-0.6,-0.584615384615384,-0.569230769230769,
-0.553846153846154,-0.538461538461538,-0.523076923076923,-0.507692307692308,
-0.492307692307692,-0.476923076923077,-0.461538461538462,-0.446153846153846,
-0.430769230769231,-0.415384615384615,-0.4,-0.384615384615385,-0.369230769230769,
-0.353846153846154,-0.338461538461538,-0.323076923076923,-0.307692307692308,
-0.292307692307692,-0.276923076923077,-0.261538461538462,-0.246153846153846,
-0.230769230769231,-0.215384615384615,-0.2,-0.184615384615385,-0.169230769230769,
-0.153846153846154,-0.138461538461538,-0.123076923076923,-0.107692307692308,
-0.0923076923076923,-0.0769230769230769,-0.0615384615384615,-0.0461538461538462,
-0.0307692307692308,-0.0153846153846154,0.),(-1.,1.),.UNSPECIFIED.)
GEOMETRIC_REPRESENTATION_ITEM()
RATIONAL_B_SPLINE_SURFACE(((1.,1.),(1.,1.),(1.,1.),(1.,1.),(1.,1.),(1.,
1.),(1.,1.),(1.,1.),(1.,1.),(1.,1.),(1.,1.),(1.,1.),(1.,1.),(1.,1.),(1.,
1.),(1.,1.),(1.,1.),(1.,1.),(1.,1.),(1.,1.),(1.,1.),(1.,1.),(1.,1.),(1.,
1.),(1.,1.),(1.,1.),(1.,1.),(1.,1.),(1.,1.),(1.,1.),(1.,1.),(1.,1.),(1.,
1.),(1.,1.),(1.,1.),(1.,1.),(1.,1.),(1.,1.),(1.,1.),(1.,1.),(1.,1.),(1.,
1.),(1.,1.),(1.,1.),(1.,1.),(1.,1.),(1.,1.),(1.,1.),(1.,1.),(1.,1.),(1.,
1.),(1.,1.),(1.,1.),(1.,1.),(1.,1.),(1.,1.),(1.,1.),(1.,1.),(1.,1.),(1.,
1.),(1.,1.),(1.,1.),(1.,1.),(1.,1.),(1.,1.),(1.,1.),(1.,1.),(1.,1.),(1.,
1.),(1.,1.)))
REPRESENTATION_ITEM('')
SURFACE()
);
#45=(
BOUNDED_SURFACE()
B_SPLINE_SURFACE(5,1,((#31120,#31121),(#31122,#31123),(#31124,#31125),(#31126,
#31127),(#31128,#31129),(#31130,#31131),(#31132,#31133),(#31134,#31135),
(#31136,#31137),(#31138,#31139),(#31140,#31141),(#31142,#31143),(#31144,
#31145),(#31146,#31147),(#31148,#31149),(#31150,#31151),(#31152,#31153),
(#31154,#31155),(#31156,#31157),(#31158,#31159),(#31160,#31161),(#31162,
#31163),(#31164,#31165),(#31166,#31167),(#31168,#31169),(#31170,#31171),
(#31172,#31173),(#31174,#31175),(#31176,#31177),(#31178,#31179),(#31180,
#31181),(#31182,#31183),(#31184,#31185),(#31186,#31187),(#31188,#31189),
(#31190,#31191),(#31192,#31193),(#31194,#31195),(#31196,#31197),(#31198,
#31199),(#31200,#31201),(#31202,#31203),(#31204,#31205),(#31206,#31207),
(#31208,#31209),(#31210,#31211),(#31212,#31213),(#31214,#31215),(#31216,
#31217),(#31218,#31219),(#31220,#31221),(#31222,#31223),(#31224,#31225),
(#31226,#31227),(#31228,#31229),(#31230,#31231),(#31232,#31233),(#31234,
#31235),(#31236,#31237),(#31238,#31239),(#31240,#31241),(#31242,#31243),
(#31244,#31245),(#31246,#31247),(#31248,#31249),(#31250,#31251),(#31252,
#31253),(#31254,#31255),(#31256,#31257),(#31258,#31259)),.UNSPECIFIED.,
 .F.,.F.,.F.)
B_SPLINE_SURFACE_WITH_KNOTS((6,1,1,1,1,1,1,1,1,1,1,1,1,1,1,1,1,1,1,1,1,
1,1,1,1,1,1,1,1,1,1,1,1,1,1,1,1,1,1,1,1,1,1,1,1,1,1,1,1,1,1,1,1,1,1,1,1,
1,1,1,1,1,1,1,1,6),(2,2),(-1.,-0.984615384615383,-0.969230769230768,-0.953846153846152,
-0.938461538461537,-0.923076923076922,-0.907692307692306,-0.892307692307691,
-0.876923076923076,-0.86153846153846,-0.846153846153845,-0.83076923076923,
-0.815384615384614,-0.799999999999999,-0.784615384615384,-0.769230769230768,
-0.753846153846153,-0.738461538461538,-0.723076923076922,-0.707692307692307,
-0.692307692307692,-0.676923076923076,-0.661538461538461,-0.646153846153846,
-0.63076923076923,-0.615384615384615,-0.6,-0.584615384615384,-0.569230769230769,
-0.553846153846154,-0.538461538461538,-0.523076923076923,-0.507692307692308,
-0.492307692307692,-0.476923076923077,-0.461538461538462,-0.446153846153846,
-0.430769230769231,-0.415384615384615,-0.4,-0.384615384615385,-0.369230769230769,
-0.353846153846154,-0.338461538461538,-0.323076923076923,-0.307692307692308,
-0.292307692307692,-0.276923076923077,-0.261538461538462,-0.246153846153846,
-0.230769230769231,-0.215384615384615,-0.2,-0.184615384615385,-0.169230769230769,
-0.153846153846154,-0.138461538461538,-0.123076923076923,-0.107692307692308,
-0.0923076923076923,-0.0769230769230769,-0.0615384615384615,-0.0461538461538462,
-0.0307692307692308,-0.0153846153846154,0.),(-1.,1.),.UNSPECIFIED.)
GEOMETRIC_REPRESENTATION_ITEM()
RATIONAL_B_SPLINE_SURFACE(((1.,1.),(1.,1.),(1.,1.),(1.,1.),(1.,1.),(1.,
1.),(1.,1.),(1.,1.),(1.,1.),(1.,1.),(1.,1.),(1.,1.),(1.,1.),(1.,1.),(1.,
1.),(1.,1.),(1.,1.),(1.,1.),(1.,1.),(1.,1.),(1.,1.),(1.,1.),(1.,1.),(1.,
1.),(1.,1.),(1.,1.),(1.,1.),(1.,1.),(1.,1.),(1.,1.),(1.,1.),(1.,1.),(1.,
1.),(1.,1.),(1.,1.),(1.,1.),(1.,1.),(1.,1.),(1.,1.),(1.,1.),(1.,1.),(1.,
1.),(1.,1.),(1.,1.),(1.,1.),(1.,1.),(1.,1.),(1.,1.),(1.,1.),(1.,1.),(1.,
1.),(1.,1.),(1.,1.),(1.,1.),(1.,1.),(1.,1.),(1.,1.),(1.,1.),(1.,1.),(1.,
1.),(1.,1.),(1.,1.),(1.,1.),(1.,1.),(1.,1.),(1.,1.),(1.,1.),(1.,1.),(1.,
1.),(1.,1.)))
REPRESENTATION_ITEM('')
SURFACE()
);
#46=(
BOUNDED_SURFACE()
B_SPLINE_SURFACE(5,1,((#31336,#31337),(#31338,#31339),(#31340,#31341),(#31342,
#31343),(#31344,#31345),(#31346,#31347),(#31348,#31349),(#31350,#31351),
(#31352,#31353),(#31354,#31355),(#31356,#31357),(#31358,#31359),(#31360,
#31361),(#31362,#31363),(#31364,#31365),(#31366,#31367),(#31368,#31369),
(#31370,#31371),(#31372,#31373),(#31374,#31375),(#31376,#31377),(#31378,
#31379),(#31380,#31381),(#31382,#31383),(#31384,#31385),(#31386,#31387),
(#31388,#31389),(#31390,#31391),(#31392,#31393),(#31394,#31395),(#31396,
#31397),(#31398,#31399),(#31400,#31401),(#31402,#31403),(#31404,#31405),
(#31406,#31407),(#31408,#31409),(#31410,#31411),(#31412,#31413),(#31414,
#31415),(#31416,#31417),(#31418,#31419),(#31420,#31421),(#31422,#31423),
(#31424,#31425),(#31426,#31427),(#31428,#31429),(#31430,#31431),(#31432,
#31433),(#31434,#31435),(#31436,#31437),(#31438,#31439),(#31440,#31441),
(#31442,#31443),(#31444,#31445),(#31446,#31447),(#31448,#31449),(#31450,
#31451),(#31452,#31453),(#31454,#31455),(#31456,#31457),(#31458,#31459),
(#31460,#31461),(#31462,#31463),(#31464,#31465),(#31466,#31467),(#31468,
#31469),(#31470,#31471),(#31472,#31473),(#31474,#31475)),.UNSPECIFIED.,
 .F.,.F.,.F.)
B_SPLINE_SURFACE_WITH_KNOTS((6,1,1,1,1,1,1,1,1,1,1,1,1,1,1,1,1,1,1,1,1,
1,1,1,1,1,1,1,1,1,1,1,1,1,1,1,1,1,1,1,1,1,1,1,1,1,1,1,1,1,1,1,1,1,1,1,1,
1,1,1,1,1,1,1,1,6),(2,2),(-1.,-0.984615384615383,-0.969230769230768,-0.953846153846152,
-0.938461538461537,-0.923076923076922,-0.907692307692306,-0.892307692307691,
-0.876923076923076,-0.86153846153846,-0.846153846153845,-0.83076923076923,
-0.815384615384614,-0.799999999999999,-0.784615384615384,-0.769230769230768,
-0.753846153846153,-0.738461538461538,-0.723076923076922,-0.707692307692307,
-0.692307692307692,-0.676923076923076,-0.661538461538461,-0.646153846153846,
-0.63076923076923,-0.615384615384615,-0.6,-0.584615384615384,-0.569230769230769,
-0.553846153846154,-0.538461538461538,-0.523076923076923,-0.507692307692308,
-0.492307692307692,-0.476923076923077,-0.461538461538462,-0.446153846153846,
-0.430769230769231,-0.415384615384615,-0.4,-0.384615384615385,-0.369230769230769,
-0.353846153846154,-0.338461538461538,-0.323076923076923,-0.307692307692308,
-0.292307692307692,-0.276923076923077,-0.261538461538462,-0.246153846153846,
-0.230769230769231,-0.215384615384615,-0.2,-0.184615384615385,-0.169230769230769,
-0.153846153846154,-0.138461538461538,-0.123076923076923,-0.107692307692308,
-0.0923076923076923,-0.0769230769230769,-0.0615384615384615,-0.0461538461538462,
-0.0307692307692308,-0.0153846153846154,0.),(-1.,1.),.UNSPECIFIED.)
GEOMETRIC_REPRESENTATION_ITEM()
RATIONAL_B_SPLINE_SURFACE(((1.,1.),(1.,1.),(1.,1.),(1.,1.),(1.,1.),(1.,
1.),(1.,1.),(1.,1.),(1.,1.),(1.,1.),(1.,1.),(1.,1.),(1.,1.),(1.,1.),(1.,
1.),(1.,1.),(1.,1.),(1.,1.),(1.,1.),(1.,1.),(1.,1.),(1.,1.),(1.,1.),(1.,
1.),(1.,1.),(1.,1.),(1.,1.),(1.,1.),(1.,1.),(1.,1.),(1.,1.),(1.,1.),(1.,
1.),(1.,1.),(1.,1.),(1.,1.),(1.,1.),(1.,1.),(1.,1.),(1.,1.),(1.,1.),(1.,
1.),(1.,1.),(1.,1.),(1.,1.),(1.,1.),(1.,1.),(1.,1.),(1.,1.),(1.,1.),(1.,
1.),(1.,1.),(1.,1.),(1.,1.),(1.,1.),(1.,1.),(1.,1.),(1.,1.),(1.,1.),(1.,
1.),(1.,1.),(1.,1.),(1.,1.),(1.,1.),(1.,1.),(1.,1.),(1.,1.),(1.,1.),(1.,
1.),(1.,1.)))
REPRESENTATION_ITEM('')
SURFACE()
);
#47=(
BOUNDED_SURFACE()
B_SPLINE_SURFACE(5,1,((#31552,#31553),(#31554,#31555),(#31556,#31557),(#31558,
#31559),(#31560,#31561),(#31562,#31563),(#31564,#31565),(#31566,#31567),
(#31568,#31569),(#31570,#31571),(#31572,#31573),(#31574,#31575),(#31576,
#31577),(#31578,#31579),(#31580,#31581),(#31582,#31583),(#31584,#31585),
(#31586,#31587),(#31588,#31589),(#31590,#31591),(#31592,#31593),(#31594,
#31595),(#31596,#31597),(#31598,#31599),(#31600,#31601),(#31602,#31603),
(#31604,#31605),(#31606,#31607),(#31608,#31609),(#31610,#31611),(#31612,
#31613),(#31614,#31615),(#31616,#31617),(#31618,#31619),(#31620,#31621),
(#31622,#31623),(#31624,#31625),(#31626,#31627),(#31628,#31629),(#31630,
#31631),(#31632,#31633),(#31634,#31635),(#31636,#31637),(#31638,#31639),
(#31640,#31641),(#31642,#31643),(#31644,#31645),(#31646,#31647),(#31648,
#31649),(#31650,#31651),(#31652,#31653),(#31654,#31655),(#31656,#31657),
(#31658,#31659),(#31660,#31661),(#31662,#31663),(#31664,#31665),(#31666,
#31667),(#31668,#31669),(#31670,#31671),(#31672,#31673),(#31674,#31675),
(#31676,#31677),(#31678,#31679),(#31680,#31681),(#31682,#31683),(#31684,
#31685),(#31686,#31687),(#31688,#31689),(#31690,#31691)),.UNSPECIFIED.,
 .F.,.F.,.F.)
B_SPLINE_SURFACE_WITH_KNOTS((6,1,1,1,1,1,1,1,1,1,1,1,1,1,1,1,1,1,1,1,1,
1,1,1,1,1,1,1,1,1,1,1,1,1,1,1,1,1,1,1,1,1,1,1,1,1,1,1,1,1,1,1,1,1,1,1,1,
1,1,1,1,1,1,1,1,6),(2,2),(-1.,-0.984615384615383,-0.969230769230768,-0.953846153846152,
-0.938461538461537,-0.923076923076922,-0.907692307692306,-0.892307692307691,
-0.876923076923076,-0.86153846153846,-0.846153846153845,-0.83076923076923,
-0.815384615384614,-0.799999999999999,-0.784615384615384,-0.769230769230768,
-0.753846153846153,-0.738461538461538,-0.723076923076922,-0.707692307692307,
-0.692307692307692,-0.676923076923076,-0.661538461538461,-0.646153846153846,
-0.63076923076923,-0.615384615384615,-0.6,-0.584615384615384,-0.569230769230769,
-0.553846153846154,-0.538461538461538,-0.523076923076923,-0.507692307692308,
-0.492307692307692,-0.476923076923077,-0.461538461538462,-0.446153846153846,
-0.430769230769231,-0.415384615384615,-0.4,-0.384615384615385,-0.369230769230769,
-0.353846153846154,-0.338461538461538,-0.323076923076923,-0.307692307692308,
-0.292307692307692,-0.276923076923077,-0.261538461538462,-0.246153846153846,
-0.230769230769231,-0.215384615384615,-0.2,-0.184615384615385,-0.169230769230769,
-0.153846153846154,-0.138461538461538,-0.123076923076923,-0.107692307692308,
-0.0923076923076923,-0.0769230769230769,-0.0615384615384615,-0.0461538461538462,
-0.0307692307692308,-0.0153846153846154,0.),(-1.,1.),.UNSPECIFIED.)
GEOMETRIC_REPRESENTATION_ITEM()
RATIONAL_B_SPLINE_SURFACE(((1.,1.),(1.,1.),(1.,1.),(1.,1.),(1.,1.),(1.,
1.),(1.,1.),(1.,1.),(1.,1.),(1.,1.),(1.,1.),(1.,1.),(1.,1.),(1.,1.),(1.,
1.),(1.,1.),(1.,1.),(1.,1.),(1.,1.),(1.,1.),(1.,1.),(1.,1.),(1.,1.),(1.,
1.),(1.,1.),(1.,1.),(1.,1.),(1.,1.),(1.,1.),(1.,1.),(1.,1.),(1.,1.),(1.,
1.),(1.,1.),(1.,1.),(1.,1.),(1.,1.),(1.,1.),(1.,1.),(1.,1.),(1.,1.),(1.,
1.),(1.,1.),(1.,1.),(1.,1.),(1.,1.),(1.,1.),(1.,1.),(1.,1.),(1.,1.),(1.,
1.),(1.,1.),(1.,1.),(1.,1.),(1.,1.),(1.,1.),(1.,1.),(1.,1.),(1.,1.),(1.,
1.),(1.,1.),(1.,1.),(1.,1.),(1.,1.),(1.,1.),(1.,1.),(1.,1.),(1.,1.),(1.,
1.),(1.,1.)))
REPRESENTATION_ITEM('')
SURFACE()
);
#48=(
BOUNDED_SURFACE()
B_SPLINE_SURFACE(5,1,((#31768,#31769),(#31770,#31771),(#31772,#31773),(#31774,
#31775),(#31776,#31777),(#31778,#31779),(#31780,#31781),(#31782,#31783),
(#31784,#31785),(#31786,#31787),(#31788,#31789),(#31790,#31791),(#31792,
#31793),(#31794,#31795),(#31796,#31797),(#31798,#31799),(#31800,#31801),
(#31802,#31803),(#31804,#31805),(#31806,#31807),(#31808,#31809),(#31810,
#31811),(#31812,#31813),(#31814,#31815),(#31816,#31817),(#31818,#31819),
(#31820,#31821),(#31822,#31823),(#31824,#31825),(#31826,#31827),(#31828,
#31829),(#31830,#31831),(#31832,#31833),(#31834,#31835),(#31836,#31837),
(#31838,#31839),(#31840,#31841),(#31842,#31843),(#31844,#31845),(#31846,
#31847),(#31848,#31849),(#31850,#31851),(#31852,#31853),(#31854,#31855),
(#31856,#31857),(#31858,#31859),(#31860,#31861),(#31862,#31863),(#31864,
#31865),(#31866,#31867),(#31868,#31869),(#31870,#31871),(#31872,#31873),
(#31874,#31875),(#31876,#31877),(#31878,#31879),(#31880,#31881),(#31882,
#31883),(#31884,#31885),(#31886,#31887),(#31888,#31889),(#31890,#31891),
(#31892,#31893),(#31894,#31895),(#31896,#31897),(#31898,#31899),(#31900,
#31901),(#31902,#31903),(#31904,#31905),(#31906,#31907)),.UNSPECIFIED.,
 .F.,.F.,.F.)
B_SPLINE_SURFACE_WITH_KNOTS((6,1,1,1,1,1,1,1,1,1,1,1,1,1,1,1,1,1,1,1,1,
1,1,1,1,1,1,1,1,1,1,1,1,1,1,1,1,1,1,1,1,1,1,1,1,1,1,1,1,1,1,1,1,1,1,1,1,
1,1,1,1,1,1,1,1,6),(2,2),(-1.,-0.984615384615383,-0.969230769230768,-0.953846153846152,
-0.938461538461537,-0.923076923076922,-0.907692307692306,-0.892307692307691,
-0.876923076923076,-0.86153846153846,-0.846153846153845,-0.83076923076923,
-0.815384615384614,-0.799999999999999,-0.784615384615384,-0.769230769230768,
-0.753846153846153,-0.738461538461538,-0.723076923076922,-0.707692307692307,
-0.692307692307692,-0.676923076923076,-0.661538461538461,-0.646153846153846,
-0.63076923076923,-0.615384615384615,-0.6,-0.584615384615384,-0.569230769230769,
-0.553846153846154,-0.538461538461538,-0.523076923076923,-0.507692307692308,
-0.492307692307692,-0.476923076923077,-0.461538461538462,-0.446153846153846,
-0.430769230769231,-0.415384615384615,-0.4,-0.384615384615385,-0.369230769230769,
-0.353846153846154,-0.338461538461538,-0.323076923076923,-0.307692307692308,
-0.292307692307692,-0.276923076923077,-0.261538461538462,-0.246153846153846,
-0.230769230769231,-0.215384615384615,-0.2,-0.184615384615385,-0.169230769230769,
-0.153846153846154,-0.138461538461538,-0.123076923076923,-0.107692307692308,
-0.0923076923076923,-0.0769230769230769,-0.0615384615384615,-0.0461538461538462,
-0.0307692307692308,-0.0153846153846154,0.),(-1.,1.),.UNSPECIFIED.)
GEOMETRIC_REPRESENTATION_ITEM()
RATIONAL_B_SPLINE_SURFACE(((1.,1.),(1.,1.),(1.,1.),(1.,1.),(1.,1.),(1.,
1.),(1.,1.),(1.,1.),(1.,1.),(1.,1.),(1.,1.),(1.,1.),(1.,1.),(1.,1.),(1.,
1.),(1.,1.),(1.,1.),(1.,1.),(1.,1.),(1.,1.),(1.,1.),(1.,1.),(1.,1.),(1.,
1.),(1.,1.),(1.,1.),(1.,1.),(1.,1.),(1.,1.),(1.,1.),(1.,1.),(1.,1.),(1.,
1.),(1.,1.),(1.,1.),(1.,1.),(1.,1.),(1.,1.),(1.,1.),(1.,1.),(1.,1.),(1.,
1.),(1.,1.),(1.,1.),(1.,1.),(1.,1.),(1.,1.),(1.,1.),(1.,1.),(1.,1.),(1.,
1.),(1.,1.),(1.,1.),(1.,1.),(1.,1.),(1.,1.),(1.,1.),(1.,1.),(1.,1.),(1.,
1.),(1.,1.),(1.,1.),(1.,1.),(1.,1.),(1.,1.),(1.,1.),(1.,1.),(1.,1.),(1.,
1.),(1.,1.)))
REPRESENTATION_ITEM('')
SURFACE()
);
#49=(
BOUNDED_SURFACE()
B_SPLINE_SURFACE(5,1,((#31984,#31985),(#31986,#31987),(#31988,#31989),(#31990,
#31991),(#31992,#31993),(#31994,#31995),(#31996,#31997),(#31998,#31999),
(#32000,#32001),(#32002,#32003),(#32004,#32005),(#32006,#32007),(#32008,
#32009),(#32010,#32011),(#32012,#32013),(#32014,#32015),(#32016,#32017),
(#32018,#32019),(#32020,#32021),(#32022,#32023),(#32024,#32025),(#32026,
#32027),(#32028,#32029),(#32030,#32031),(#32032,#32033),(#32034,#32035),
(#32036,#32037),(#32038,#32039),(#32040,#32041),(#32042,#32043),(#32044,
#32045),(#32046,#32047),(#32048,#32049),(#32050,#32051),(#32052,#32053),
(#32054,#32055),(#32056,#32057),(#32058,#32059),(#32060,#32061),(#32062,
#32063),(#32064,#32065),(#32066,#32067),(#32068,#32069),(#32070,#32071),
(#32072,#32073),(#32074,#32075),(#32076,#32077),(#32078,#32079),(#32080,
#32081),(#32082,#32083),(#32084,#32085),(#32086,#32087),(#32088,#32089),
(#32090,#32091),(#32092,#32093),(#32094,#32095),(#32096,#32097),(#32098,
#32099),(#32100,#32101),(#32102,#32103),(#32104,#32105),(#32106,#32107),
(#32108,#32109),(#32110,#32111),(#32112,#32113),(#32114,#32115),(#32116,
#32117),(#32118,#32119),(#32120,#32121),(#32122,#32123)),.UNSPECIFIED.,
 .F.,.F.,.F.)
B_SPLINE_SURFACE_WITH_KNOTS((6,1,1,1,1,1,1,1,1,1,1,1,1,1,1,1,1,1,1,1,1,
1,1,1,1,1,1,1,1,1,1,1,1,1,1,1,1,1,1,1,1,1,1,1,1,1,1,1,1,1,1,1,1,1,1,1,1,
1,1,1,1,1,1,1,1,6),(2,2),(-1.,-0.984615384615383,-0.969230769230768,-0.953846153846152,
-0.938461538461537,-0.923076923076922,-0.907692307692306,-0.892307692307691,
-0.876923076923076,-0.86153846153846,-0.846153846153845,-0.83076923076923,
-0.815384615384614,-0.799999999999999,-0.784615384615384,-0.769230769230768,
-0.753846153846153,-0.738461538461538,-0.723076923076922,-0.707692307692307,
-0.692307692307692,-0.676923076923076,-0.661538461538461,-0.646153846153846,
-0.63076923076923,-0.615384615384615,-0.6,-0.584615384615384,-0.569230769230769,
-0.553846153846154,-0.538461538461538,-0.523076923076923,-0.507692307692308,
-0.492307692307692,-0.476923076923077,-0.461538461538462,-0.446153846153846,
-0.430769230769231,-0.415384615384615,-0.4,-0.384615384615385,-0.369230769230769,
-0.353846153846154,-0.338461538461538,-0.323076923076923,-0.307692307692308,
-0.292307692307692,-0.276923076923077,-0.261538461538462,-0.246153846153846,
-0.230769230769231,-0.215384615384615,-0.2,-0.184615384615385,-0.169230769230769,
-0.153846153846154,-0.138461538461538,-0.123076923076923,-0.107692307692308,
-0.0923076923076923,-0.0769230769230769,-0.0615384615384615,-0.0461538461538462,
-0.0307692307692308,-0.0153846153846154,0.),(-1.,1.),.UNSPECIFIED.)
GEOMETRIC_REPRESENTATION_ITEM()
RATIONAL_B_SPLINE_SURFACE(((1.,1.),(1.,1.),(1.,1.),(1.,1.),(1.,1.),(1.,
1.),(1.,1.),(1.,1.),(1.,1.),(1.,1.),(1.,1.),(1.,1.),(1.,1.),(1.,1.),(1.,
1.),(1.,1.),(1.,1.),(1.,1.),(1.,1.),(1.,1.),(1.,1.),(1.,1.),(1.,1.),(1.,
1.),(1.,1.),(1.,1.),(1.,1.),(1.,1.),(1.,1.),(1.,1.),(1.,1.),(1.,1.),(1.,
1.),(1.,1.),(1.,1.),(1.,1.),(1.,1.),(1.,1.),(1.,1.),(1.,1.),(1.,1.),(1.,
1.),(1.,1.),(1.,1.),(1.,1.),(1.,1.),(1.,1.),(1.,1.),(1.,1.),(1.,1.),(1.,
1.),(1.,1.),(1.,1.),(1.,1.),(1.,1.),(1.,1.),(1.,1.),(1.,1.),(1.,1.),(1.,
1.),(1.,1.),(1.,1.),(1.,1.),(1.,1.),(1.,1.),(1.,1.),(1.,1.),(1.,1.),(1.,
1.),(1.,1.)))
REPRESENTATION_ITEM('')
SURFACE()
);
#50=(
BOUNDED_SURFACE()
B_SPLINE_SURFACE(5,1,((#32200,#32201),(#32202,#32203),(#32204,#32205),(#32206,
#32207),(#32208,#32209),(#32210,#32211),(#32212,#32213),(#32214,#32215),
(#32216,#32217),(#32218,#32219),(#32220,#32221),(#32222,#32223),(#32224,
#32225),(#32226,#32227),(#32228,#32229),(#32230,#32231),(#32232,#32233),
(#32234,#32235),(#32236,#32237),(#32238,#32239),(#32240,#32241),(#32242,
#32243),(#32244,#32245),(#32246,#32247),(#32248,#32249),(#32250,#32251),
(#32252,#32253),(#32254,#32255),(#32256,#32257),(#32258,#32259),(#32260,
#32261),(#32262,#32263),(#32264,#32265),(#32266,#32267),(#32268,#32269),
(#32270,#32271),(#32272,#32273),(#32274,#32275),(#32276,#32277),(#32278,
#32279),(#32280,#32281),(#32282,#32283),(#32284,#32285),(#32286,#32287),
(#32288,#32289),(#32290,#32291),(#32292,#32293),(#32294,#32295),(#32296,
#32297),(#32298,#32299),(#32300,#32301),(#32302,#32303),(#32304,#32305),
(#32306,#32307),(#32308,#32309),(#32310,#32311),(#32312,#32313),(#32314,
#32315),(#32316,#32317),(#32318,#32319),(#32320,#32321),(#32322,#32323),
(#32324,#32325),(#32326,#32327),(#32328,#32329),(#32330,#32331),(#32332,
#32333),(#32334,#32335),(#32336,#32337),(#32338,#32339)),.UNSPECIFIED.,
 .F.,.F.,.F.)
B_SPLINE_SURFACE_WITH_KNOTS((6,1,1,1,1,1,1,1,1,1,1,1,1,1,1,1,1,1,1,1,1,
1,1,1,1,1,1,1,1,1,1,1,1,1,1,1,1,1,1,1,1,1,1,1,1,1,1,1,1,1,1,1,1,1,1,1,1,
1,1,1,1,1,1,1,1,6),(2,2),(-1.,-0.984615384615383,-0.969230769230768,-0.953846153846152,
-0.938461538461537,-0.923076923076922,-0.907692307692306,-0.892307692307691,
-0.876923076923076,-0.86153846153846,-0.846153846153845,-0.83076923076923,
-0.815384615384614,-0.799999999999999,-0.784615384615384,-0.769230769230768,
-0.753846153846153,-0.738461538461538,-0.723076923076922,-0.707692307692307,
-0.692307692307692,-0.676923076923076,-0.661538461538461,-0.646153846153846,
-0.63076923076923,-0.615384615384615,-0.6,-0.584615384615384,-0.569230769230769,
-0.553846153846154,-0.538461538461538,-0.523076923076923,-0.507692307692308,
-0.492307692307692,-0.476923076923077,-0.461538461538462,-0.446153846153846,
-0.430769230769231,-0.415384615384615,-0.4,-0.384615384615385,-0.369230769230769,
-0.353846153846154,-0.338461538461538,-0.323076923076923,-0.307692307692308,
-0.292307692307692,-0.276923076923077,-0.261538461538462,-0.246153846153846,
-0.230769230769231,-0.215384615384615,-0.2,-0.184615384615385,-0.169230769230769,
-0.153846153846154,-0.138461538461538,-0.123076923076923,-0.107692307692308,
-0.0923076923076923,-0.0769230769230769,-0.0615384615384615,-0.0461538461538462,
-0.0307692307692308,-0.0153846153846154,0.),(-1.,1.),.UNSPECIFIED.)
GEOMETRIC_REPRESENTATION_ITEM()
RATIONAL_B_SPLINE_SURFACE(((1.,1.),(1.,1.),(1.,1.),(1.,1.),(1.,1.),(1.,
1.),(1.,1.),(1.,1.),(1.,1.),(1.,1.),(1.,1.),(1.,1.),(1.,1.),(1.,1.),(1.,
1.),(1.,1.),(1.,1.),(1.,1.),(1.,1.),(1.,1.),(1.,1.),(1.,1.),(1.,1.),(1.,
1.),(1.,1.),(1.,1.),(1.,1.),(1.,1.),(1.,1.),(1.,1.),(1.,1.),(1.,1.),(1.,
1.),(1.,1.),(1.,1.),(1.,1.),(1.,1.),(1.,1.),(1.,1.),(1.,1.),(1.,1.),(1.,
1.),(1.,1.),(1.,1.),(1.,1.),(1.,1.),(1.,1.),(1.,1.),(1.,1.),(1.,1.),(1.,
1.),(1.,1.),(1.,1.),(1.,1.),(1.,1.),(1.,1.),(1.,1.),(1.,1.),(1.,1.),(1.,
1.),(1.,1.),(1.,1.),(1.,1.),(1.,1.),(1.,1.),(1.,1.),(1.,1.),(1.,1.),(1.,
1.),(1.,1.)))
REPRESENTATION_ITEM('')
SURFACE()
);
#51=(
BOUNDED_CURVE()
B_SPLINE_CURVE(5,(#20848,#20849,#20850,#20851,#20852,#20853,#20854,#20855,
#20856,#20857,#20858,#20859,#20860,#20861,#20862,#20863,#20864,#20865,#20866,
#20867,#20868,#20869,#20870,#20871,#20872,#20873,#20874,#20875,#20876,#20877,
#20878,#20879,#20880,#20881,#20882,#20883,#20884,#20885,#20886,#20887,#20888,
#20889,#20890,#20891,#20892,#20893,#20894,#20895,#20896,#20897,#20898,#20899,
#20900,#20901,#20902,#20903,#20904,#20905,#20906,#20907,#20908,#20909,#20910,
#20911,#20912,#20913,#20914,#20915,#20916,#20917),.UNSPECIFIED.,.F.,.F.)
B_SPLINE_CURVE_WITH_KNOTS((6,1,1,1,1,1,1,1,1,1,1,1,1,1,1,1,1,1,1,1,1,1,
1,1,1,1,1,1,1,1,1,1,1,1,1,1,1,1,1,1,1,1,1,1,1,1,1,1,1,1,1,1,1,1,1,1,1,1,
1,1,1,1,1,1,1,6),(0.,0.0153846153846154,0.0307692307692308,0.0461538461538462,
0.0615384615384615,0.0769230769230769,0.0923076923076923,0.107692307692308,
0.123076923076923,0.138461538461538,0.153846153846154,0.169230769230769,
0.184615384615385,0.2,0.215384615384615,0.230769230769231,0.246153846153846,
0.261538461538462,0.276923076923077,0.292307692307692,0.307692307692308,
0.323076923076923,0.338461538461538,0.353846153846154,0.369230769230769,
0.384615384615385,0.4,0.415384615384615,0.430769230769231,0.446153846153846,
0.461538461538462,0.476923076923077,0.492307692307692,0.507692307692308,
0.523076923076923,0.538461538461538,0.553846153846154,0.569230769230769,
0.584615384615384,0.6,0.615384615384615,0.63076923076923,0.646153846153846,
0.661538461538461,0.676923076923076,0.692307692307692,0.707692307692307,
0.723076923076922,0.738461538461538,0.753846153846153,0.769230769230768,
0.784615384615384,0.799999999999999,0.815384615384614,0.83076923076923,
0.846153846153845,0.86153846153846,0.876923076923076,0.892307692307691,
0.907692307692306,0.923076923076922,0.938461538461537,0.953846153846152,
0.969230769230768,0.984615384615383,1.),.UNSPECIFIED.)
CURVE()
GEOMETRIC_REPRESENTATION_ITEM()
RATIONAL_B_SPLINE_CURVE((1.,1.,1.,1.,1.,1.,1.,1.,1.,1.,1.,1.,1.,1.,1.,1.,
1.,1.,1.,1.,1.,1.,1.,1.,1.,1.,1.,1.,1.,1.,1.,1.,1.,1.,1.,1.,1.,1.,1.,1.,
1.,1.,1.,1.,1.,1.,1.,1.,1.,1.,1.,1.,1.,1.,1.,1.,1.,1.,1.,1.,1.,1.,1.,1.,
1.,1.,1.,1.,1.,1.))
REPRESENTATION_ITEM('')
);
#52=(
BOUNDED_CURVE()
B_SPLINE_CURVE(5,(#20921,#20922,#20923,#20924,#20925,#20926,#20927,#20928,
#20929,#20930,#20931,#20932,#20933,#20934,#20935,#20936,#20937,#20938,#20939,
#20940,#20941,#20942,#20943,#20944,#20945,#20946,#20947,#20948,#20949,#20950,
#20951,#20952,#20953,#20954,#20955,#20956,#20957,#20958,#20959,#20960,#20961,
#20962,#20963,#20964,#20965,#20966,#20967,#20968,#20969,#20970,#20971,#20972,
#20973,#20974,#20975,#20976,#20977,#20978,#20979,#20980,#20981,#20982,#20983,
#20984,#20985,#20986,#20987,#20988,#20989,#20990),.UNSPECIFIED.,.F.,.F.)
B_SPLINE_CURVE_WITH_KNOTS((6,1,1,1,1,1,1,1,1,1,1,1,1,1,1,1,1,1,1,1,1,1,
1,1,1,1,1,1,1,1,1,1,1,1,1,1,1,1,1,1,1,1,1,1,1,1,1,1,1,1,1,1,1,1,1,1,1,1,
1,1,1,1,1,1,1,6),(0.,0.0153846153846154,0.0307692307692308,0.0461538461538462,
0.0615384615384615,0.0769230769230769,0.0923076923076923,0.107692307692308,
0.123076923076923,0.138461538461538,0.153846153846154,0.169230769230769,
0.184615384615385,0.2,0.215384615384615,0.230769230769231,0.246153846153846,
0.261538461538462,0.276923076923077,0.292307692307692,0.307692307692308,
0.323076923076923,0.338461538461538,0.353846153846154,0.369230769230769,
0.384615384615385,0.4,0.415384615384615,0.430769230769231,0.446153846153846,
0.461538461538462,0.476923076923077,0.492307692307692,0.507692307692308,
0.523076923076923,0.538461538461538,0.553846153846154,0.569230769230769,
0.584615384615384,0.6,0.615384615384615,0.63076923076923,0.646153846153846,
0.661538461538461,0.676923076923076,0.692307692307692,0.707692307692307,
0.723076923076922,0.738461538461538,0.753846153846153,0.769230769230768,
0.784615384615384,0.799999999999999,0.815384615384614,0.83076923076923,
0.846153846153845,0.86153846153846,0.876923076923076,0.892307692307691,
0.907692307692306,0.923076923076922,0.938461538461537,0.953846153846152,
0.969230769230768,0.984615384615383,1.),.UNSPECIFIED.)
CURVE()
GEOMETRIC_REPRESENTATION_ITEM()
RATIONAL_B_SPLINE_CURVE((1.,1.,1.,1.,1.,1.,1.,1.,1.,1.,1.,1.,1.,1.,1.,1.,
1.,1.,1.,1.,1.,1.,1.,1.,1.,1.,1.,1.,1.,1.,1.,1.,1.,1.,1.,1.,1.,1.,1.,1.,
1.,1.,1.,1.,1.,1.,1.,1.,1.,1.,1.,1.,1.,1.,1.,1.,1.,1.,1.,1.,1.,1.,1.,1.,
1.,1.,1.,1.,1.,1.))
REPRESENTATION_ITEM('')
);
#53=(
BOUNDED_CURVE()
B_SPLINE_CURVE(5,(#20994,#20995,#20996,#20997,#20998,#20999,#21000,#21001,
#21002,#21003,#21004,#21005,#21006,#21007,#21008,#21009,#21010,#21011,#21012,
#21013,#21014,#21015,#21016,#21017,#21018,#21019,#21020,#21021,#21022,#21023,
#21024,#21025,#21026,#21027,#21028,#21029,#21030,#21031,#21032,#21033,#21034,
#21035,#21036,#21037,#21038,#21039,#21040,#21041,#21042,#21043,#21044,#21045,
#21046,#21047,#21048,#21049,#21050,#21051,#21052,#21053,#21054,#21055,#21056,
#21057,#21058,#21059,#21060,#21061,#21062,#21063),.UNSPECIFIED.,.F.,.F.)
B_SPLINE_CURVE_WITH_KNOTS((6,1,1,1,1,1,1,1,1,1,1,1,1,1,1,1,1,1,1,1,1,1,
1,1,1,1,1,1,1,1,1,1,1,1,1,1,1,1,1,1,1,1,1,1,1,1,1,1,1,1,1,1,1,1,1,1,1,1,
1,1,1,1,1,1,1,6),(0.,0.0153846153846154,0.0307692307692308,0.0461538461538462,
0.0615384615384615,0.0769230769230769,0.0923076923076923,0.107692307692308,
0.123076923076923,0.138461538461538,0.153846153846154,0.169230769230769,
0.184615384615385,0.2,0.215384615384615,0.230769230769231,0.246153846153846,
0.261538461538462,0.276923076923077,0.292307692307692,0.307692307692308,
0.323076923076923,0.338461538461538,0.353846153846154,0.369230769230769,
0.384615384615385,0.4,0.415384615384615,0.430769230769231,0.446153846153846,
0.461538461538462,0.476923076923077,0.492307692307692,0.507692307692308,
0.523076923076923,0.538461538461538,0.553846153846154,0.569230769230769,
0.584615384615384,0.6,0.615384615384615,0.63076923076923,0.646153846153846,
0.661538461538461,0.676923076923076,0.692307692307692,0.707692307692307,
0.723076923076922,0.738461538461538,0.753846153846153,0.769230769230768,
0.784615384615384,0.799999999999999,0.815384615384614,0.83076923076923,
0.846153846153845,0.86153846153846,0.876923076923076,0.892307692307691,
0.907692307692306,0.923076923076922,0.938461538461537,0.953846153846152,
0.969230769230768,0.984615384615383,1.),.UNSPECIFIED.)
CURVE()
GEOMETRIC_REPRESENTATION_ITEM()
RATIONAL_B_SPLINE_CURVE((1.,1.,1.,1.,1.,1.,1.,1.,1.,1.,1.,1.,1.,1.,1.,1.,
1.,1.,1.,1.,1.,1.,1.,1.,1.,1.,1.,1.,1.,1.,1.,1.,1.,1.,1.,1.,1.,1.,1.,1.,
1.,1.,1.,1.,1.,1.,1.,1.,1.,1.,1.,1.,1.,1.,1.,1.,1.,1.,1.,1.,1.,1.,1.,1.,
1.,1.,1.,1.,1.,1.))
REPRESENTATION_ITEM('')
);
#54=(
BOUNDED_CURVE()
B_SPLINE_CURVE(5,(#21067,#21068,#21069,#21070,#21071,#21072,#21073,#21074,
#21075,#21076,#21077,#21078,#21079,#21080,#21081,#21082,#21083,#21084,#21085,
#21086,#21087,#21088,#21089,#21090,#21091,#21092,#21093,#21094,#21095,#21096,
#21097,#21098,#21099,#21100,#21101,#21102,#21103,#21104,#21105,#21106,#21107,
#21108,#21109,#21110,#21111,#21112,#21113,#21114,#21115,#21116,#21117,#21118,
#21119,#21120,#21121,#21122,#21123,#21124,#21125,#21126,#21127,#21128,#21129,
#21130,#21131,#21132,#21133,#21134,#21135,#21136),.UNSPECIFIED.,.F.,.F.)
B_SPLINE_CURVE_WITH_KNOTS((6,1,1,1,1,1,1,1,1,1,1,1,1,1,1,1,1,1,1,1,1,1,
1,1,1,1,1,1,1,1,1,1,1,1,1,1,1,1,1,1,1,1,1,1,1,1,1,1,1,1,1,1,1,1,1,1,1,1,
1,1,1,1,1,1,1,6),(0.,0.0153846153846154,0.0307692307692308,0.0461538461538462,
0.0615384615384615,0.0769230769230769,0.0923076923076923,0.107692307692308,
0.123076923076923,0.138461538461538,0.153846153846154,0.169230769230769,
0.184615384615385,0.2,0.215384615384615,0.230769230769231,0.246153846153846,
0.261538461538462,0.276923076923077,0.292307692307692,0.307692307692308,
0.323076923076923,0.338461538461538,0.353846153846154,0.369230769230769,
0.384615384615385,0.4,0.415384615384615,0.430769230769231,0.446153846153846,
0.461538461538462,0.476923076923077,0.492307692307692,0.507692307692308,
0.523076923076923,0.538461538461538,0.553846153846154,0.569230769230769,
0.584615384615384,0.6,0.615384615384615,0.63076923076923,0.646153846153846,
0.661538461538461,0.676923076923076,0.692307692307692,0.707692307692307,
0.723076923076922,0.738461538461538,0.753846153846153,0.769230769230768,
0.784615384615384,0.799999999999999,0.815384615384614,0.83076923076923,
0.846153846153845,0.86153846153846,0.876923076923076,0.892307692307691,
0.907692307692306,0.923076923076922,0.938461538461537,0.953846153846152,
0.969230769230768,0.984615384615383,1.),.UNSPECIFIED.)
CURVE()
GEOMETRIC_REPRESENTATION_ITEM()
RATIONAL_B_SPLINE_CURVE((1.,1.,1.,1.,1.,1.,1.,1.,1.,1.,1.,1.,1.,1.,1.,1.,
1.,1.,1.,1.,1.,1.,1.,1.,1.,1.,1.,1.,1.,1.,1.,1.,1.,1.,1.,1.,1.,1.,1.,1.,
1.,1.,1.,1.,1.,1.,1.,1.,1.,1.,1.,1.,1.,1.,1.,1.,1.,1.,1.,1.,1.,1.,1.,1.,
1.,1.,1.,1.,1.,1.))
REPRESENTATION_ITEM('')
);
#55=(
BOUNDED_CURVE()
B_SPLINE_CURVE(5,(#21140,#21141,#21142,#21143,#21144,#21145,#21146,#21147,
#21148,#21149,#21150,#21151,#21152,#21153,#21154,#21155,#21156,#21157,#21158,
#21159,#21160,#21161,#21162,#21163,#21164,#21165,#21166,#21167,#21168,#21169,
#21170,#21171,#21172,#21173,#21174,#21175,#21176,#21177,#21178,#21179,#21180,
#21181,#21182,#21183,#21184,#21185,#21186,#21187,#21188,#21189,#21190,#21191,
#21192,#21193,#21194,#21195,#21196,#21197,#21198,#21199,#21200,#21201,#21202,
#21203,#21204,#21205,#21206,#21207,#21208,#21209),.UNSPECIFIED.,.F.,.F.)
B_SPLINE_CURVE_WITH_KNOTS((6,1,1,1,1,1,1,1,1,1,1,1,1,1,1,1,1,1,1,1,1,1,
1,1,1,1,1,1,1,1,1,1,1,1,1,1,1,1,1,1,1,1,1,1,1,1,1,1,1,1,1,1,1,1,1,1,1,1,
1,1,1,1,1,1,1,6),(0.,0.0153846153846154,0.0307692307692308,0.0461538461538462,
0.0615384615384615,0.0769230769230769,0.0923076923076923,0.107692307692308,
0.123076923076923,0.138461538461538,0.153846153846154,0.169230769230769,
0.184615384615385,0.2,0.215384615384615,0.230769230769231,0.246153846153846,
0.261538461538462,0.276923076923077,0.292307692307692,0.307692307692308,
0.323076923076923,0.338461538461538,0.353846153846154,0.369230769230769,
0.384615384615385,0.4,0.415384615384615,0.430769230769231,0.446153846153846,
0.461538461538462,0.476923076923077,0.492307692307692,0.507692307692308,
0.523076923076923,0.538461538461538,0.553846153846154,0.569230769230769,
0.584615384615384,0.6,0.615384615384615,0.63076923076923,0.646153846153846,
0.661538461538461,0.676923076923076,0.692307692307692,0.707692307692307,
0.723076923076922,0.738461538461538,0.753846153846153,0.769230769230768,
0.784615384615384,0.799999999999999,0.815384615384614,0.83076923076923,
0.846153846153845,0.86153846153846,0.876923076923076,0.892307692307691,
0.907692307692306,0.923076923076922,0.938461538461537,0.953846153846152,
0.969230769230768,0.984615384615383,1.),.UNSPECIFIED.)
CURVE()
GEOMETRIC_REPRESENTATION_ITEM()
RATIONAL_B_SPLINE_CURVE((1.,1.,1.,1.,1.,1.,1.,1.,1.,1.,1.,1.,1.,1.,1.,1.,
1.,1.,1.,1.,1.,1.,1.,1.,1.,1.,1.,1.,1.,1.,1.,1.,1.,1.,1.,1.,1.,1.,1.,1.,
1.,1.,1.,1.,1.,1.,1.,1.,1.,1.,1.,1.,1.,1.,1.,1.,1.,1.,1.,1.,1.,1.,1.,1.,
1.,1.,1.,1.,1.,1.))
REPRESENTATION_ITEM('')
);
#56=(
BOUNDED_CURVE()
B_SPLINE_CURVE(5,(#21213,#21214,#21215,#21216,#21217,#21218,#21219,#21220,
#21221,#21222,#21223,#21224,#21225,#21226,#21227,#21228,#21229,#21230,#21231,
#21232,#21233,#21234,#21235,#21236,#21237,#21238,#21239,#21240,#21241,#21242,
#21243,#21244,#21245,#21246,#21247,#21248,#21249,#21250,#21251,#21252,#21253,
#21254,#21255,#21256,#21257,#21258,#21259,#21260,#21261,#21262,#21263,#21264,
#21265,#21266,#21267,#21268,#21269,#21270,#21271,#21272,#21273,#21274,#21275,
#21276,#21277,#21278,#21279,#21280,#21281,#21282),.UNSPECIFIED.,.F.,.F.)
B_SPLINE_CURVE_WITH_KNOTS((6,1,1,1,1,1,1,1,1,1,1,1,1,1,1,1,1,1,1,1,1,1,
1,1,1,1,1,1,1,1,1,1,1,1,1,1,1,1,1,1,1,1,1,1,1,1,1,1,1,1,1,1,1,1,1,1,1,1,
1,1,1,1,1,1,1,6),(0.,0.0153846153846154,0.0307692307692308,0.0461538461538462,
0.0615384615384615,0.0769230769230769,0.0923076923076923,0.107692307692308,
0.123076923076923,0.138461538461538,0.153846153846154,0.169230769230769,
0.184615384615385,0.2,0.215384615384615,0.230769230769231,0.246153846153846,
0.261538461538462,0.276923076923077,0.292307692307692,0.307692307692308,
0.323076923076923,0.338461538461538,0.353846153846154,0.369230769230769,
0.384615384615385,0.4,0.415384615384615,0.430769230769231,0.446153846153846,
0.461538461538462,0.476923076923077,0.492307692307692,0.507692307692308,
0.523076923076923,0.538461538461538,0.553846153846154,0.569230769230769,
0.584615384615384,0.6,0.615384615384615,0.63076923076923,0.646153846153846,
0.661538461538461,0.676923076923076,0.692307692307692,0.707692307692307,
0.723076923076922,0.738461538461538,0.753846153846153,0.769230769230768,
0.784615384615384,0.799999999999999,0.815384615384614,0.83076923076923,
0.846153846153845,0.86153846153846,0.876923076923076,0.892307692307691,
0.907692307692306,0.923076923076922,0.938461538461537,0.953846153846152,
0.969230769230768,0.984615384615383,1.),.UNSPECIFIED.)
CURVE()
GEOMETRIC_REPRESENTATION_ITEM()
RATIONAL_B_SPLINE_CURVE((1.,1.,1.,1.,1.,1.,1.,1.,1.,1.,1.,1.,1.,1.,1.,1.,
1.,1.,1.,1.,1.,1.,1.,1.,1.,1.,1.,1.,1.,1.,1.,1.,1.,1.,1.,1.,1.,1.,1.,1.,
1.,1.,1.,1.,1.,1.,1.,1.,1.,1.,1.,1.,1.,1.,1.,1.,1.,1.,1.,1.,1.,1.,1.,1.,
1.,1.,1.,1.,1.,1.))
REPRESENTATION_ITEM('')
);
#57=(
BOUNDED_CURVE()
B_SPLINE_CURVE(5,(#21286,#21287,#21288,#21289,#21290,#21291,#21292,#21293,
#21294,#21295,#21296,#21297,#21298,#21299,#21300,#21301,#21302,#21303,#21304,
#21305,#21306,#21307,#21308,#21309,#21310,#21311,#21312,#21313,#21314,#21315,
#21316,#21317,#21318,#21319,#21320,#21321,#21322,#21323,#21324,#21325,#21326,
#21327,#21328,#21329,#21330,#21331,#21332,#21333,#21334,#21335,#21336,#21337,
#21338,#21339,#21340,#21341,#21342,#21343,#21344,#21345,#21346,#21347,#21348,
#21349,#21350,#21351,#21352,#21353,#21354,#21355),.UNSPECIFIED.,.F.,.F.)
B_SPLINE_CURVE_WITH_KNOTS((6,1,1,1,1,1,1,1,1,1,1,1,1,1,1,1,1,1,1,1,1,1,
1,1,1,1,1,1,1,1,1,1,1,1,1,1,1,1,1,1,1,1,1,1,1,1,1,1,1,1,1,1,1,1,1,1,1,1,
1,1,1,1,1,1,1,6),(0.,0.0153846153846154,0.0307692307692308,0.0461538461538462,
0.0615384615384615,0.0769230769230769,0.0923076923076923,0.107692307692308,
0.123076923076923,0.138461538461538,0.153846153846154,0.169230769230769,
0.184615384615385,0.2,0.215384615384615,0.230769230769231,0.246153846153846,
0.261538461538462,0.276923076923077,0.292307692307692,0.307692307692308,
0.323076923076923,0.338461538461538,0.353846153846154,0.369230769230769,
0.384615384615385,0.4,0.415384615384615,0.430769230769231,0.446153846153846,
0.461538461538462,0.476923076923077,0.492307692307692,0.507692307692308,
0.523076923076923,0.538461538461538,0.553846153846154,0.569230769230769,
0.584615384615384,0.6,0.615384615384615,0.63076923076923,0.646153846153846,
0.661538461538461,0.676923076923076,0.692307692307692,0.707692307692307,
0.723076923076922,0.738461538461538,0.753846153846153,0.769230769230768,
0.784615384615384,0.799999999999999,0.815384615384614,0.83076923076923,
0.846153846153845,0.86153846153846,0.876923076923076,0.892307692307691,
0.907692307692306,0.923076923076922,0.938461538461537,0.953846153846152,
0.969230769230768,0.984615384615383,1.),.UNSPECIFIED.)
CURVE()
GEOMETRIC_REPRESENTATION_ITEM()
RATIONAL_B_SPLINE_CURVE((1.,1.,1.,1.,1.,1.,1.,1.,1.,1.,1.,1.,1.,1.,1.,1.,
1.,1.,1.,1.,1.,1.,1.,1.,1.,1.,1.,1.,1.,1.,1.,1.,1.,1.,1.,1.,1.,1.,1.,1.,
1.,1.,1.,1.,1.,1.,1.,1.,1.,1.,1.,1.,1.,1.,1.,1.,1.,1.,1.,1.,1.,1.,1.,1.,
1.,1.,1.,1.,1.,1.))
REPRESENTATION_ITEM('')
);
#58=(
BOUNDED_CURVE()
B_SPLINE_CURVE(5,(#21359,#21360,#21361,#21362,#21363,#21364,#21365,#21366,
#21367,#21368,#21369,#21370,#21371,#21372,#21373,#21374,#21375,#21376,#21377,
#21378,#21379,#21380,#21381,#21382,#21383,#21384,#21385,#21386,#21387,#21388,
#21389,#21390,#21391,#21392,#21393,#21394,#21395,#21396,#21397,#21398,#21399,
#21400,#21401,#21402,#21403,#21404,#21405,#21406,#21407,#21408,#21409,#21410,
#21411,#21412,#21413,#21414,#21415,#21416,#21417,#21418,#21419,#21420,#21421,
#21422,#21423,#21424,#21425,#21426,#21427,#21428),.UNSPECIFIED.,.F.,.F.)
B_SPLINE_CURVE_WITH_KNOTS((6,1,1,1,1,1,1,1,1,1,1,1,1,1,1,1,1,1,1,1,1,1,
1,1,1,1,1,1,1,1,1,1,1,1,1,1,1,1,1,1,1,1,1,1,1,1,1,1,1,1,1,1,1,1,1,1,1,1,
1,1,1,1,1,1,1,6),(0.,0.0153846153846154,0.0307692307692308,0.0461538461538462,
0.0615384615384615,0.0769230769230769,0.0923076923076923,0.107692307692308,
0.123076923076923,0.138461538461538,0.153846153846154,0.169230769230769,
0.184615384615385,0.2,0.215384615384615,0.230769230769231,0.246153846153846,
0.261538461538462,0.276923076923077,0.292307692307692,0.307692307692308,
0.323076923076923,0.338461538461538,0.353846153846154,0.369230769230769,
0.384615384615385,0.4,0.415384615384615,0.430769230769231,0.446153846153846,
0.461538461538462,0.476923076923077,0.492307692307692,0.507692307692308,
0.523076923076923,0.538461538461538,0.553846153846154,0.569230769230769,
0.584615384615384,0.6,0.615384615384615,0.63076923076923,0.646153846153846,
0.661538461538461,0.676923076923076,0.692307692307692,0.707692307692307,
0.723076923076922,0.738461538461538,0.753846153846153,0.769230769230768,
0.784615384615384,0.799999999999999,0.815384615384614,0.83076923076923,
0.846153846153845,0.86153846153846,0.876923076923076,0.892307692307691,
0.907692307692306,0.923076923076922,0.938461538461537,0.953846153846152,
0.969230769230768,0.984615384615383,1.),.UNSPECIFIED.)
CURVE()
GEOMETRIC_REPRESENTATION_ITEM()
RATIONAL_B_SPLINE_CURVE((1.,1.,1.,1.,1.,1.,1.,1.,1.,1.,1.,1.,1.,1.,1.,1.,
1.,1.,1.,1.,1.,1.,1.,1.,1.,1.,1.,1.,1.,1.,1.,1.,1.,1.,1.,1.,1.,1.,1.,1.,
1.,1.,1.,1.,1.,1.,1.,1.,1.,1.,1.,1.,1.,1.,1.,1.,1.,1.,1.,1.,1.,1.,1.,1.,
1.,1.,1.,1.,1.,1.))
REPRESENTATION_ITEM('')
);
#59=(
BOUNDED_CURVE()
B_SPLINE_CURVE(5,(#21432,#21433,#21434,#21435,#21436,#21437,#21438,#21439,
#21440,#21441,#21442,#21443,#21444,#21445,#21446,#21447,#21448,#21449,#21450,
#21451,#21452,#21453,#21454,#21455,#21456,#21457,#21458,#21459,#21460,#21461,
#21462,#21463,#21464,#21465,#21466,#21467,#21468,#21469,#21470,#21471,#21472,
#21473,#21474,#21475,#21476,#21477,#21478,#21479,#21480,#21481,#21482,#21483,
#21484,#21485,#21486,#21487,#21488,#21489,#21490,#21491,#21492,#21493,#21494,
#21495,#21496,#21497,#21498,#21499,#21500,#21501),.UNSPECIFIED.,.F.,.F.)
B_SPLINE_CURVE_WITH_KNOTS((6,1,1,1,1,1,1,1,1,1,1,1,1,1,1,1,1,1,1,1,1,1,
1,1,1,1,1,1,1,1,1,1,1,1,1,1,1,1,1,1,1,1,1,1,1,1,1,1,1,1,1,1,1,1,1,1,1,1,
1,1,1,1,1,1,1,6),(0.,0.0153846153846154,0.0307692307692308,0.0461538461538462,
0.0615384615384615,0.0769230769230769,0.0923076923076923,0.107692307692308,
0.123076923076923,0.138461538461538,0.153846153846154,0.169230769230769,
0.184615384615385,0.2,0.215384615384615,0.230769230769231,0.246153846153846,
0.261538461538462,0.276923076923077,0.292307692307692,0.307692307692308,
0.323076923076923,0.338461538461538,0.353846153846154,0.369230769230769,
0.384615384615385,0.4,0.415384615384615,0.430769230769231,0.446153846153846,
0.461538461538462,0.476923076923077,0.492307692307692,0.507692307692308,
0.523076923076923,0.538461538461538,0.553846153846154,0.569230769230769,
0.584615384615384,0.6,0.615384615384615,0.63076923076923,0.646153846153846,
0.661538461538461,0.676923076923076,0.692307692307692,0.707692307692307,
0.723076923076922,0.738461538461538,0.753846153846153,0.769230769230768,
0.784615384615384,0.799999999999999,0.815384615384614,0.83076923076923,
0.846153846153845,0.86153846153846,0.876923076923076,0.892307692307691,
0.907692307692306,0.923076923076922,0.938461538461537,0.953846153846152,
0.969230769230768,0.984615384615383,1.),.UNSPECIFIED.)
CURVE()
GEOMETRIC_REPRESENTATION_ITEM()
RATIONAL_B_SPLINE_CURVE((1.,1.,1.,1.,1.,1.,1.,1.,1.,1.,1.,1.,1.,1.,1.,1.,
1.,1.,1.,1.,1.,1.,1.,1.,1.,1.,1.,1.,1.,1.,1.,1.,1.,1.,1.,1.,1.,1.,1.,1.,
1.,1.,1.,1.,1.,1.,1.,1.,1.,1.,1.,1.,1.,1.,1.,1.,1.,1.,1.,1.,1.,1.,1.,1.,
1.,1.,1.,1.,1.,1.))
REPRESENTATION_ITEM('')
);
#60=(
BOUNDED_CURVE()
B_SPLINE_CURVE(5,(#21505,#21506,#21507,#21508,#21509,#21510,#21511,#21512,
#21513,#21514,#21515,#21516,#21517,#21518,#21519,#21520,#21521,#21522,#21523,
#21524,#21525,#21526,#21527,#21528,#21529,#21530,#21531,#21532,#21533,#21534,
#21535,#21536,#21537,#21538,#21539,#21540,#21541,#21542,#21543,#21544,#21545,
#21546,#21547,#21548,#21549,#21550,#21551,#21552,#21553,#21554,#21555,#21556,
#21557,#21558,#21559,#21560,#21561,#21562,#21563,#21564,#21565,#21566,#21567,
#21568,#21569,#21570,#21571,#21572,#21573,#21574),.UNSPECIFIED.,.F.,.F.)
B_SPLINE_CURVE_WITH_KNOTS((6,1,1,1,1,1,1,1,1,1,1,1,1,1,1,1,1,1,1,1,1,1,
1,1,1,1,1,1,1,1,1,1,1,1,1,1,1,1,1,1,1,1,1,1,1,1,1,1,1,1,1,1,1,1,1,1,1,1,
1,1,1,1,1,1,1,6),(0.,0.0153846153846154,0.0307692307692308,0.0461538461538462,
0.0615384615384615,0.0769230769230769,0.0923076923076923,0.107692307692308,
0.123076923076923,0.138461538461538,0.153846153846154,0.169230769230769,
0.184615384615385,0.2,0.215384615384615,0.230769230769231,0.246153846153846,
0.261538461538462,0.276923076923077,0.292307692307692,0.307692307692308,
0.323076923076923,0.338461538461538,0.353846153846154,0.369230769230769,
0.384615384615385,0.4,0.415384615384615,0.430769230769231,0.446153846153846,
0.461538461538462,0.476923076923077,0.492307692307692,0.507692307692308,
0.523076923076923,0.538461538461538,0.553846153846154,0.569230769230769,
0.584615384615384,0.6,0.615384615384615,0.63076923076923,0.646153846153846,
0.661538461538461,0.676923076923076,0.692307692307692,0.707692307692307,
0.723076923076922,0.738461538461538,0.753846153846153,0.769230769230768,
0.784615384615384,0.799999999999999,0.815384615384614,0.83076923076923,
0.846153846153845,0.86153846153846,0.876923076923076,0.892307692307691,
0.907692307692306,0.923076923076922,0.938461538461537,0.953846153846152,
0.969230769230768,0.984615384615383,1.),.UNSPECIFIED.)
CURVE()
GEOMETRIC_REPRESENTATION_ITEM()
RATIONAL_B_SPLINE_CURVE((1.,1.,1.,1.,1.,1.,1.,1.,1.,1.,1.,1.,1.,1.,1.,1.,
1.,1.,1.,1.,1.,1.,1.,1.,1.,1.,1.,1.,1.,1.,1.,1.,1.,1.,1.,1.,1.,1.,1.,1.,
1.,1.,1.,1.,1.,1.,1.,1.,1.,1.,1.,1.,1.,1.,1.,1.,1.,1.,1.,1.,1.,1.,1.,1.,
1.,1.,1.,1.,1.,1.))
REPRESENTATION_ITEM('')
);
#61=(
BOUNDED_CURVE()
B_SPLINE_CURVE(5,(#21578,#21579,#21580,#21581,#21582,#21583,#21584,#21585,
#21586,#21587,#21588,#21589,#21590,#21591,#21592,#21593,#21594,#21595,#21596,
#21597,#21598,#21599,#21600,#21601,#21602,#21603,#21604,#21605,#21606,#21607,
#21608,#21609,#21610,#21611,#21612,#21613,#21614,#21615,#21616,#21617,#21618,
#21619,#21620,#21621,#21622,#21623,#21624,#21625,#21626,#21627,#21628,#21629,
#21630,#21631,#21632,#21633,#21634,#21635,#21636,#21637,#21638,#21639,#21640,
#21641,#21642,#21643,#21644,#21645,#21646,#21647),.UNSPECIFIED.,.F.,.F.)
B_SPLINE_CURVE_WITH_KNOTS((6,1,1,1,1,1,1,1,1,1,1,1,1,1,1,1,1,1,1,1,1,1,
1,1,1,1,1,1,1,1,1,1,1,1,1,1,1,1,1,1,1,1,1,1,1,1,1,1,1,1,1,1,1,1,1,1,1,1,
1,1,1,1,1,1,1,6),(0.,0.0153846153846154,0.0307692307692308,0.0461538461538462,
0.0615384615384615,0.0769230769230769,0.0923076923076923,0.107692307692308,
0.123076923076923,0.138461538461538,0.153846153846154,0.169230769230769,
0.184615384615385,0.2,0.215384615384615,0.230769230769231,0.246153846153846,
0.261538461538462,0.276923076923077,0.292307692307692,0.307692307692308,
0.323076923076923,0.338461538461538,0.353846153846154,0.369230769230769,
0.384615384615385,0.4,0.415384615384615,0.430769230769231,0.446153846153846,
0.461538461538462,0.476923076923077,0.492307692307692,0.507692307692308,
0.523076923076923,0.538461538461538,0.553846153846154,0.569230769230769,
0.584615384615384,0.6,0.615384615384615,0.63076923076923,0.646153846153846,
0.661538461538461,0.676923076923076,0.692307692307692,0.707692307692307,
0.723076923076922,0.738461538461538,0.753846153846153,0.769230769230768,
0.784615384615384,0.799999999999999,0.815384615384614,0.83076923076923,
0.846153846153845,0.86153846153846,0.876923076923076,0.892307692307691,
0.907692307692306,0.923076923076922,0.938461538461537,0.953846153846152,
0.969230769230768,0.984615384615383,1.),.UNSPECIFIED.)
CURVE()
GEOMETRIC_REPRESENTATION_ITEM()
RATIONAL_B_SPLINE_CURVE((1.,1.,1.,1.,1.,1.,1.,1.,1.,1.,1.,1.,1.,1.,1.,1.,
1.,1.,1.,1.,1.,1.,1.,1.,1.,1.,1.,1.,1.,1.,1.,1.,1.,1.,1.,1.,1.,1.,1.,1.,
1.,1.,1.,1.,1.,1.,1.,1.,1.,1.,1.,1.,1.,1.,1.,1.,1.,1.,1.,1.,1.,1.,1.,1.,
1.,1.,1.,1.,1.,1.))
REPRESENTATION_ITEM('')
);
#62=(
BOUNDED_CURVE()
B_SPLINE_CURVE(5,(#21651,#21652,#21653,#21654,#21655,#21656,#21657,#21658,
#21659,#21660,#21661,#21662,#21663,#21664,#21665,#21666,#21667,#21668,#21669,
#21670,#21671,#21672,#21673,#21674,#21675,#21676,#21677,#21678,#21679,#21680,
#21681,#21682,#21683,#21684,#21685,#21686,#21687,#21688,#21689,#21690,#21691,
#21692,#21693,#21694,#21695,#21696,#21697,#21698,#21699,#21700,#21701,#21702,
#21703,#21704,#21705,#21706,#21707,#21708,#21709,#21710,#21711,#21712,#21713,
#21714,#21715,#21716,#21717,#21718,#21719,#21720),.UNSPECIFIED.,.F.,.F.)
B_SPLINE_CURVE_WITH_KNOTS((6,1,1,1,1,1,1,1,1,1,1,1,1,1,1,1,1,1,1,1,1,1,
1,1,1,1,1,1,1,1,1,1,1,1,1,1,1,1,1,1,1,1,1,1,1,1,1,1,1,1,1,1,1,1,1,1,1,1,
1,1,1,1,1,1,1,6),(0.,0.0153846153846154,0.0307692307692308,0.0461538461538462,
0.0615384615384615,0.0769230769230769,0.0923076923076923,0.107692307692308,
0.123076923076923,0.138461538461538,0.153846153846154,0.169230769230769,
0.184615384615385,0.2,0.215384615384615,0.230769230769231,0.246153846153846,
0.261538461538462,0.276923076923077,0.292307692307692,0.307692307692308,
0.323076923076923,0.338461538461538,0.353846153846154,0.369230769230769,
0.384615384615385,0.4,0.415384615384615,0.430769230769231,0.446153846153846,
0.461538461538462,0.476923076923077,0.492307692307692,0.507692307692308,
0.523076923076923,0.538461538461538,0.553846153846154,0.569230769230769,
0.584615384615384,0.6,0.615384615384615,0.63076923076923,0.646153846153846,
0.661538461538461,0.676923076923076,0.692307692307692,0.707692307692307,
0.723076923076922,0.738461538461538,0.753846153846153,0.769230769230768,
0.784615384615384,0.799999999999999,0.815384615384614,0.83076923076923,
0.846153846153845,0.86153846153846,0.876923076923076,0.892307692307691,
0.907692307692306,0.923076923076922,0.938461538461537,0.953846153846152,
0.969230769230768,0.984615384615383,1.),.UNSPECIFIED.)
CURVE()
GEOMETRIC_REPRESENTATION_ITEM()
RATIONAL_B_SPLINE_CURVE((1.,1.,1.,1.,1.,1.,1.,1.,1.,1.,1.,1.,1.,1.,1.,1.,
1.,1.,1.,1.,1.,1.,1.,1.,1.,1.,1.,1.,1.,1.,1.,1.,1.,1.,1.,1.,1.,1.,1.,1.,
1.,1.,1.,1.,1.,1.,1.,1.,1.,1.,1.,1.,1.,1.,1.,1.,1.,1.,1.,1.,1.,1.,1.,1.,
1.,1.,1.,1.,1.,1.))
REPRESENTATION_ITEM('')
);
#63=(
BOUNDED_CURVE()
B_SPLINE_CURVE(5,(#21724,#21725,#21726,#21727,#21728,#21729,#21730,#21731,
#21732,#21733,#21734,#21735,#21736,#21737,#21738,#21739,#21740,#21741,#21742,
#21743,#21744,#21745,#21746,#21747,#21748,#21749,#21750,#21751,#21752,#21753,
#21754,#21755,#21756,#21757,#21758,#21759,#21760,#21761,#21762,#21763,#21764,
#21765,#21766,#21767,#21768,#21769,#21770,#21771,#21772,#21773,#21774,#21775,
#21776,#21777,#21778,#21779,#21780,#21781,#21782,#21783,#21784,#21785,#21786,
#21787,#21788,#21789,#21790,#21791,#21792,#21793),.UNSPECIFIED.,.F.,.F.)
B_SPLINE_CURVE_WITH_KNOTS((6,1,1,1,1,1,1,1,1,1,1,1,1,1,1,1,1,1,1,1,1,1,
1,1,1,1,1,1,1,1,1,1,1,1,1,1,1,1,1,1,1,1,1,1,1,1,1,1,1,1,1,1,1,1,1,1,1,1,
1,1,1,1,1,1,1,6),(0.,0.0153846153846154,0.0307692307692308,0.0461538461538462,
0.0615384615384615,0.0769230769230769,0.0923076923076923,0.107692307692308,
0.123076923076923,0.138461538461538,0.153846153846154,0.169230769230769,
0.184615384615385,0.2,0.215384615384615,0.230769230769231,0.246153846153846,
0.261538461538462,0.276923076923077,0.292307692307692,0.307692307692308,
0.323076923076923,0.338461538461538,0.353846153846154,0.369230769230769,
0.384615384615385,0.4,0.415384615384615,0.430769230769231,0.446153846153846,
0.461538461538462,0.476923076923077,0.492307692307692,0.507692307692308,
0.523076923076923,0.538461538461538,0.553846153846154,0.569230769230769,
0.584615384615384,0.6,0.615384615384615,0.63076923076923,0.646153846153846,
0.661538461538461,0.676923076923076,0.692307692307692,0.707692307692307,
0.723076923076922,0.738461538461538,0.753846153846153,0.769230769230768,
0.784615384615384,0.799999999999999,0.815384615384614,0.83076923076923,
0.846153846153845,0.86153846153846,0.876923076923076,0.892307692307691,
0.907692307692306,0.923076923076922,0.938461538461537,0.953846153846152,
0.969230769230768,0.984615384615383,1.),.UNSPECIFIED.)
CURVE()
GEOMETRIC_REPRESENTATION_ITEM()
RATIONAL_B_SPLINE_CURVE((1.,1.,1.,1.,1.,1.,1.,1.,1.,1.,1.,1.,1.,1.,1.,1.,
1.,1.,1.,1.,1.,1.,1.,1.,1.,1.,1.,1.,1.,1.,1.,1.,1.,1.,1.,1.,1.,1.,1.,1.,
1.,1.,1.,1.,1.,1.,1.,1.,1.,1.,1.,1.,1.,1.,1.,1.,1.,1.,1.,1.,1.,1.,1.,1.,
1.,1.,1.,1.,1.,1.))
REPRESENTATION_ITEM('')
);
#64=(
BOUNDED_CURVE()
B_SPLINE_CURVE(5,(#21797,#21798,#21799,#21800,#21801,#21802,#21803,#21804,
#21805,#21806,#21807,#21808,#21809,#21810,#21811,#21812,#21813,#21814,#21815,
#21816,#21817,#21818,#21819,#21820,#21821,#21822,#21823,#21824,#21825,#21826,
#21827,#21828,#21829,#21830,#21831,#21832,#21833,#21834,#21835,#21836,#21837,
#21838,#21839,#21840,#21841,#21842,#21843,#21844,#21845,#21846,#21847,#21848,
#21849,#21850,#21851,#21852,#21853,#21854,#21855,#21856,#21857,#21858,#21859,
#21860,#21861,#21862,#21863,#21864,#21865,#21866),.UNSPECIFIED.,.F.,.F.)
B_SPLINE_CURVE_WITH_KNOTS((6,1,1,1,1,1,1,1,1,1,1,1,1,1,1,1,1,1,1,1,1,1,
1,1,1,1,1,1,1,1,1,1,1,1,1,1,1,1,1,1,1,1,1,1,1,1,1,1,1,1,1,1,1,1,1,1,1,1,
1,1,1,1,1,1,1,6),(0.,0.0153846153846154,0.0307692307692308,0.0461538461538462,
0.0615384615384615,0.0769230769230769,0.0923076923076923,0.107692307692308,
0.123076923076923,0.138461538461538,0.153846153846154,0.169230769230769,
0.184615384615385,0.2,0.215384615384615,0.230769230769231,0.246153846153846,
0.261538461538462,0.276923076923077,0.292307692307692,0.307692307692308,
0.323076923076923,0.338461538461538,0.353846153846154,0.369230769230769,
0.384615384615385,0.4,0.415384615384615,0.430769230769231,0.446153846153846,
0.461538461538462,0.476923076923077,0.492307692307692,0.507692307692308,
0.523076923076923,0.538461538461538,0.553846153846154,0.569230769230769,
0.584615384615384,0.6,0.615384615384615,0.63076923076923,0.646153846153846,
0.661538461538461,0.676923076923076,0.692307692307692,0.707692307692307,
0.723076923076922,0.738461538461538,0.753846153846153,0.769230769230768,
0.784615384615384,0.799999999999999,0.815384615384614,0.83076923076923,
0.846153846153845,0.86153846153846,0.876923076923076,0.892307692307691,
0.907692307692306,0.923076923076922,0.938461538461537,0.953846153846152,
0.969230769230768,0.984615384615383,1.),.UNSPECIFIED.)
CURVE()
GEOMETRIC_REPRESENTATION_ITEM()
RATIONAL_B_SPLINE_CURVE((1.,1.,1.,1.,1.,1.,1.,1.,1.,1.,1.,1.,1.,1.,1.,1.,
1.,1.,1.,1.,1.,1.,1.,1.,1.,1.,1.,1.,1.,1.,1.,1.,1.,1.,1.,1.,1.,1.,1.,1.,
1.,1.,1.,1.,1.,1.,1.,1.,1.,1.,1.,1.,1.,1.,1.,1.,1.,1.,1.,1.,1.,1.,1.,1.,
1.,1.,1.,1.,1.,1.))
REPRESENTATION_ITEM('')
);
#65=(
BOUNDED_CURVE()
B_SPLINE_CURVE(5,(#21870,#21871,#21872,#21873,#21874,#21875,#21876,#21877,
#21878,#21879,#21880,#21881,#21882,#21883,#21884,#21885,#21886,#21887,#21888,
#21889,#21890,#21891,#21892,#21893,#21894,#21895,#21896,#21897,#21898,#21899,
#21900,#21901,#21902,#21903,#21904,#21905,#21906,#21907,#21908,#21909,#21910,
#21911,#21912,#21913,#21914,#21915,#21916,#21917,#21918,#21919,#21920,#21921,
#21922,#21923,#21924,#21925,#21926,#21927,#21928,#21929,#21930,#21931,#21932,
#21933,#21934,#21935,#21936,#21937,#21938,#21939),.UNSPECIFIED.,.F.,.F.)
B_SPLINE_CURVE_WITH_KNOTS((6,1,1,1,1,1,1,1,1,1,1,1,1,1,1,1,1,1,1,1,1,1,
1,1,1,1,1,1,1,1,1,1,1,1,1,1,1,1,1,1,1,1,1,1,1,1,1,1,1,1,1,1,1,1,1,1,1,1,
1,1,1,1,1,1,1,6),(0.,0.0153846153846154,0.0307692307692308,0.0461538461538462,
0.0615384615384615,0.0769230769230769,0.0923076923076923,0.107692307692308,
0.123076923076923,0.138461538461538,0.153846153846154,0.169230769230769,
0.184615384615385,0.2,0.215384615384615,0.230769230769231,0.246153846153846,
0.261538461538462,0.276923076923077,0.292307692307692,0.307692307692308,
0.323076923076923,0.338461538461538,0.353846153846154,0.369230769230769,
0.384615384615385,0.4,0.415384615384615,0.430769230769231,0.446153846153846,
0.461538461538462,0.476923076923077,0.492307692307692,0.507692307692308,
0.523076923076923,0.538461538461538,0.553846153846154,0.569230769230769,
0.584615384615384,0.6,0.615384615384615,0.63076923076923,0.646153846153846,
0.661538461538461,0.676923076923076,0.692307692307692,0.707692307692307,
0.723076923076922,0.738461538461538,0.753846153846153,0.769230769230768,
0.784615384615384,0.799999999999999,0.815384615384614,0.83076923076923,
0.846153846153845,0.86153846153846,0.876923076923076,0.892307692307691,
0.907692307692306,0.923076923076922,0.938461538461537,0.953846153846152,
0.969230769230768,0.984615384615383,1.),.UNSPECIFIED.)
CURVE()
GEOMETRIC_REPRESENTATION_ITEM()
RATIONAL_B_SPLINE_CURVE((1.,1.,1.,1.,1.,1.,1.,1.,1.,1.,1.,1.,1.,1.,1.,1.,
1.,1.,1.,1.,1.,1.,1.,1.,1.,1.,1.,1.,1.,1.,1.,1.,1.,1.,1.,1.,1.,1.,1.,1.,
1.,1.,1.,1.,1.,1.,1.,1.,1.,1.,1.,1.,1.,1.,1.,1.,1.,1.,1.,1.,1.,1.,1.,1.,
1.,1.,1.,1.,1.,1.))
REPRESENTATION_ITEM('')
);
#66=(
BOUNDED_CURVE()
B_SPLINE_CURVE(5,(#21943,#21944,#21945,#21946,#21947,#21948,#21949,#21950,
#21951,#21952,#21953,#21954,#21955,#21956,#21957,#21958,#21959,#21960,#21961,
#21962,#21963,#21964,#21965,#21966,#21967,#21968,#21969,#21970,#21971,#21972,
#21973,#21974,#21975,#21976,#21977,#21978,#21979,#21980,#21981,#21982,#21983,
#21984,#21985,#21986,#21987,#21988,#21989,#21990,#21991,#21992,#21993,#21994,
#21995,#21996,#21997,#21998,#21999,#22000,#22001,#22002,#22003,#22004,#22005,
#22006,#22007,#22008,#22009,#22010,#22011,#22012),.UNSPECIFIED.,.F.,.F.)
B_SPLINE_CURVE_WITH_KNOTS((6,1,1,1,1,1,1,1,1,1,1,1,1,1,1,1,1,1,1,1,1,1,
1,1,1,1,1,1,1,1,1,1,1,1,1,1,1,1,1,1,1,1,1,1,1,1,1,1,1,1,1,1,1,1,1,1,1,1,
1,1,1,1,1,1,1,6),(0.,0.0153846153846154,0.0307692307692308,0.0461538461538462,
0.0615384615384615,0.0769230769230769,0.0923076923076923,0.107692307692308,
0.123076923076923,0.138461538461538,0.153846153846154,0.169230769230769,
0.184615384615385,0.2,0.215384615384615,0.230769230769231,0.246153846153846,
0.261538461538462,0.276923076923077,0.292307692307692,0.307692307692308,
0.323076923076923,0.338461538461538,0.353846153846154,0.369230769230769,
0.384615384615385,0.4,0.415384615384615,0.430769230769231,0.446153846153846,
0.461538461538462,0.476923076923077,0.492307692307692,0.507692307692308,
0.523076923076923,0.538461538461538,0.553846153846154,0.569230769230769,
0.584615384615384,0.6,0.615384615384615,0.63076923076923,0.646153846153846,
0.661538461538461,0.676923076923076,0.692307692307692,0.707692307692307,
0.723076923076922,0.738461538461538,0.753846153846153,0.769230769230768,
0.784615384615384,0.799999999999999,0.815384615384614,0.83076923076923,
0.846153846153845,0.86153846153846,0.876923076923076,0.892307692307691,
0.907692307692306,0.923076923076922,0.938461538461537,0.953846153846152,
0.969230769230768,0.984615384615383,1.),.UNSPECIFIED.)
CURVE()
GEOMETRIC_REPRESENTATION_ITEM()
RATIONAL_B_SPLINE_CURVE((1.,1.,1.,1.,1.,1.,1.,1.,1.,1.,1.,1.,1.,1.,1.,1.,
1.,1.,1.,1.,1.,1.,1.,1.,1.,1.,1.,1.,1.,1.,1.,1.,1.,1.,1.,1.,1.,1.,1.,1.,
1.,1.,1.,1.,1.,1.,1.,1.,1.,1.,1.,1.,1.,1.,1.,1.,1.,1.,1.,1.,1.,1.,1.,1.,
1.,1.,1.,1.,1.,1.))
REPRESENTATION_ITEM('')
);
#67=(
BOUNDED_CURVE()
B_SPLINE_CURVE(5,(#22016,#22017,#22018,#22019,#22020,#22021,#22022,#22023,
#22024,#22025,#22026,#22027,#22028,#22029,#22030,#22031,#22032,#22033,#22034,
#22035,#22036,#22037,#22038,#22039,#22040,#22041,#22042,#22043,#22044,#22045,
#22046,#22047,#22048,#22049,#22050,#22051,#22052,#22053,#22054,#22055,#22056,
#22057,#22058,#22059,#22060,#22061,#22062,#22063,#22064,#22065,#22066,#22067,
#22068,#22069,#22070,#22071,#22072,#22073,#22074,#22075,#22076,#22077,#22078,
#22079,#22080,#22081,#22082,#22083,#22084,#22085),.UNSPECIFIED.,.F.,.F.)
B_SPLINE_CURVE_WITH_KNOTS((6,1,1,1,1,1,1,1,1,1,1,1,1,1,1,1,1,1,1,1,1,1,
1,1,1,1,1,1,1,1,1,1,1,1,1,1,1,1,1,1,1,1,1,1,1,1,1,1,1,1,1,1,1,1,1,1,1,1,
1,1,1,1,1,1,1,6),(0.,0.0153846153846154,0.0307692307692308,0.0461538461538462,
0.0615384615384615,0.0769230769230769,0.0923076923076923,0.107692307692308,
0.123076923076923,0.138461538461538,0.153846153846154,0.169230769230769,
0.184615384615385,0.2,0.215384615384615,0.230769230769231,0.246153846153846,
0.261538461538462,0.276923076923077,0.292307692307692,0.307692307692308,
0.323076923076923,0.338461538461538,0.353846153846154,0.369230769230769,
0.384615384615385,0.4,0.415384615384615,0.430769230769231,0.446153846153846,
0.461538461538462,0.476923076923077,0.492307692307692,0.507692307692308,
0.523076923076923,0.538461538461538,0.553846153846154,0.569230769230769,
0.584615384615384,0.6,0.615384615384615,0.63076923076923,0.646153846153846,
0.661538461538461,0.676923076923076,0.692307692307692,0.707692307692307,
0.723076923076922,0.738461538461538,0.753846153846153,0.769230769230768,
0.784615384615384,0.799999999999999,0.815384615384614,0.83076923076923,
0.846153846153845,0.86153846153846,0.876923076923076,0.892307692307691,
0.907692307692306,0.923076923076922,0.938461538461537,0.953846153846152,
0.969230769230768,0.984615384615383,1.),.UNSPECIFIED.)
CURVE()
GEOMETRIC_REPRESENTATION_ITEM()
RATIONAL_B_SPLINE_CURVE((1.,1.,1.,1.,1.,1.,1.,1.,1.,1.,1.,1.,1.,1.,1.,1.,
1.,1.,1.,1.,1.,1.,1.,1.,1.,1.,1.,1.,1.,1.,1.,1.,1.,1.,1.,1.,1.,1.,1.,1.,
1.,1.,1.,1.,1.,1.,1.,1.,1.,1.,1.,1.,1.,1.,1.,1.,1.,1.,1.,1.,1.,1.,1.,1.,
1.,1.,1.,1.,1.,1.))
REPRESENTATION_ITEM('')
);
#68=(
BOUNDED_CURVE()
B_SPLINE_CURVE(5,(#22089,#22090,#22091,#22092,#22093,#22094,#22095,#22096,
#22097,#22098,#22099,#22100,#22101,#22102,#22103,#22104,#22105,#22106,#22107,
#22108,#22109,#22110,#22111,#22112,#22113,#22114,#22115,#22116,#22117,#22118,
#22119,#22120,#22121,#22122,#22123,#22124,#22125,#22126,#22127,#22128,#22129,
#22130,#22131,#22132,#22133,#22134,#22135,#22136,#22137,#22138,#22139,#22140,
#22141,#22142,#22143,#22144,#22145,#22146,#22147,#22148,#22149,#22150,#22151,
#22152,#22153,#22154,#22155,#22156,#22157,#22158),.UNSPECIFIED.,.F.,.F.)
B_SPLINE_CURVE_WITH_KNOTS((6,1,1,1,1,1,1,1,1,1,1,1,1,1,1,1,1,1,1,1,1,1,
1,1,1,1,1,1,1,1,1,1,1,1,1,1,1,1,1,1,1,1,1,1,1,1,1,1,1,1,1,1,1,1,1,1,1,1,
1,1,1,1,1,1,1,6),(0.,0.0153846153846154,0.0307692307692308,0.0461538461538462,
0.0615384615384615,0.0769230769230769,0.0923076923076923,0.107692307692308,
0.123076923076923,0.138461538461538,0.153846153846154,0.169230769230769,
0.184615384615385,0.2,0.215384615384615,0.230769230769231,0.246153846153846,
0.261538461538462,0.276923076923077,0.292307692307692,0.307692307692308,
0.323076923076923,0.338461538461538,0.353846153846154,0.369230769230769,
0.384615384615385,0.4,0.415384615384615,0.430769230769231,0.446153846153846,
0.461538461538462,0.476923076923077,0.492307692307692,0.507692307692308,
0.523076923076923,0.538461538461538,0.553846153846154,0.569230769230769,
0.584615384615384,0.6,0.615384615384615,0.63076923076923,0.646153846153846,
0.661538461538461,0.676923076923076,0.692307692307692,0.707692307692307,
0.723076923076922,0.738461538461538,0.753846153846153,0.769230769230768,
0.784615384615384,0.799999999999999,0.815384615384614,0.83076923076923,
0.846153846153845,0.86153846153846,0.876923076923076,0.892307692307691,
0.907692307692306,0.923076923076922,0.938461538461537,0.953846153846152,
0.969230769230768,0.984615384615383,1.),.UNSPECIFIED.)
CURVE()
GEOMETRIC_REPRESENTATION_ITEM()
RATIONAL_B_SPLINE_CURVE((1.,1.,1.,1.,1.,1.,1.,1.,1.,1.,1.,1.,1.,1.,1.,1.,
1.,1.,1.,1.,1.,1.,1.,1.,1.,1.,1.,1.,1.,1.,1.,1.,1.,1.,1.,1.,1.,1.,1.,1.,
1.,1.,1.,1.,1.,1.,1.,1.,1.,1.,1.,1.,1.,1.,1.,1.,1.,1.,1.,1.,1.,1.,1.,1.,
1.,1.,1.,1.,1.,1.))
REPRESENTATION_ITEM('')
);
#69=(
BOUNDED_CURVE()
B_SPLINE_CURVE(5,(#22162,#22163,#22164,#22165,#22166,#22167,#22168,#22169,
#22170,#22171,#22172,#22173,#22174,#22175,#22176,#22177,#22178,#22179,#22180,
#22181,#22182,#22183,#22184,#22185,#22186,#22187,#22188,#22189,#22190,#22191,
#22192,#22193,#22194,#22195,#22196,#22197,#22198,#22199,#22200,#22201,#22202,
#22203,#22204,#22205,#22206,#22207,#22208,#22209,#22210,#22211,#22212,#22213,
#22214,#22215,#22216,#22217,#22218,#22219,#22220,#22221,#22222,#22223,#22224,
#22225,#22226,#22227,#22228,#22229,#22230,#22231),.UNSPECIFIED.,.F.,.F.)
B_SPLINE_CURVE_WITH_KNOTS((6,1,1,1,1,1,1,1,1,1,1,1,1,1,1,1,1,1,1,1,1,1,
1,1,1,1,1,1,1,1,1,1,1,1,1,1,1,1,1,1,1,1,1,1,1,1,1,1,1,1,1,1,1,1,1,1,1,1,
1,1,1,1,1,1,1,6),(0.,0.0153846153846154,0.0307692307692308,0.0461538461538462,
0.0615384615384615,0.0769230769230769,0.0923076923076923,0.107692307692308,
0.123076923076923,0.138461538461538,0.153846153846154,0.169230769230769,
0.184615384615385,0.2,0.215384615384615,0.230769230769231,0.246153846153846,
0.261538461538462,0.276923076923077,0.292307692307692,0.307692307692308,
0.323076923076923,0.338461538461538,0.353846153846154,0.369230769230769,
0.384615384615385,0.4,0.415384615384615,0.430769230769231,0.446153846153846,
0.461538461538462,0.476923076923077,0.492307692307692,0.507692307692308,
0.523076923076923,0.538461538461538,0.553846153846154,0.569230769230769,
0.584615384615384,0.6,0.615384615384615,0.63076923076923,0.646153846153846,
0.661538461538461,0.676923076923076,0.692307692307692,0.707692307692307,
0.723076923076922,0.738461538461538,0.753846153846153,0.769230769230768,
0.784615384615384,0.799999999999999,0.815384615384614,0.83076923076923,
0.846153846153845,0.86153846153846,0.876923076923076,0.892307692307691,
0.907692307692306,0.923076923076922,0.938461538461537,0.953846153846152,
0.969230769230768,0.984615384615383,1.),.UNSPECIFIED.)
CURVE()
GEOMETRIC_REPRESENTATION_ITEM()
RATIONAL_B_SPLINE_CURVE((1.,1.,1.,1.,1.,1.,1.,1.,1.,1.,1.,1.,1.,1.,1.,1.,
1.,1.,1.,1.,1.,1.,1.,1.,1.,1.,1.,1.,1.,1.,1.,1.,1.,1.,1.,1.,1.,1.,1.,1.,
1.,1.,1.,1.,1.,1.,1.,1.,1.,1.,1.,1.,1.,1.,1.,1.,1.,1.,1.,1.,1.,1.,1.,1.,
1.,1.,1.,1.,1.,1.))
REPRESENTATION_ITEM('')
);
#70=(
BOUNDED_CURVE()
B_SPLINE_CURVE(5,(#22235,#22236,#22237,#22238,#22239,#22240,#22241,#22242,
#22243,#22244,#22245,#22246,#22247,#22248,#22249,#22250,#22251,#22252,#22253,
#22254,#22255,#22256,#22257,#22258,#22259,#22260,#22261,#22262,#22263,#22264,
#22265,#22266,#22267,#22268,#22269,#22270,#22271,#22272,#22273,#22274,#22275,
#22276,#22277,#22278,#22279,#22280,#22281,#22282,#22283,#22284,#22285,#22286,
#22287,#22288,#22289,#22290,#22291,#22292,#22293,#22294,#22295,#22296,#22297,
#22298,#22299,#22300,#22301,#22302,#22303,#22304),.UNSPECIFIED.,.F.,.F.)
B_SPLINE_CURVE_WITH_KNOTS((6,1,1,1,1,1,1,1,1,1,1,1,1,1,1,1,1,1,1,1,1,1,
1,1,1,1,1,1,1,1,1,1,1,1,1,1,1,1,1,1,1,1,1,1,1,1,1,1,1,1,1,1,1,1,1,1,1,1,
1,1,1,1,1,1,1,6),(0.,0.0153846153846154,0.0307692307692308,0.0461538461538462,
0.0615384615384615,0.0769230769230769,0.0923076923076923,0.107692307692308,
0.123076923076923,0.138461538461538,0.153846153846154,0.169230769230769,
0.184615384615385,0.2,0.215384615384615,0.230769230769231,0.246153846153846,
0.261538461538462,0.276923076923077,0.292307692307692,0.307692307692308,
0.323076923076923,0.338461538461538,0.353846153846154,0.369230769230769,
0.384615384615385,0.4,0.415384615384615,0.430769230769231,0.446153846153846,
0.461538461538462,0.476923076923077,0.492307692307692,0.507692307692308,
0.523076923076923,0.538461538461538,0.553846153846154,0.569230769230769,
0.584615384615384,0.6,0.615384615384615,0.63076923076923,0.646153846153846,
0.661538461538461,0.676923076923076,0.692307692307692,0.707692307692307,
0.723076923076922,0.738461538461538,0.753846153846153,0.769230769230768,
0.784615384615384,0.799999999999999,0.815384615384614,0.83076923076923,
0.846153846153845,0.86153846153846,0.876923076923076,0.892307692307691,
0.907692307692306,0.923076923076922,0.938461538461537,0.953846153846152,
0.969230769230768,0.984615384615383,1.),.UNSPECIFIED.)
CURVE()
GEOMETRIC_REPRESENTATION_ITEM()
RATIONAL_B_SPLINE_CURVE((1.,1.,1.,1.,1.,1.,1.,1.,1.,1.,1.,1.,1.,1.,1.,1.,
1.,1.,1.,1.,1.,1.,1.,1.,1.,1.,1.,1.,1.,1.,1.,1.,1.,1.,1.,1.,1.,1.,1.,1.,
1.,1.,1.,1.,1.,1.,1.,1.,1.,1.,1.,1.,1.,1.,1.,1.,1.,1.,1.,1.,1.,1.,1.,1.,
1.,1.,1.,1.,1.,1.))
REPRESENTATION_ITEM('')
);
#71=(
BOUNDED_CURVE()
B_SPLINE_CURVE(5,(#22308,#22309,#22310,#22311,#22312,#22313,#22314,#22315,
#22316,#22317,#22318,#22319,#22320,#22321,#22322,#22323,#22324,#22325,#22326,
#22327,#22328,#22329,#22330,#22331,#22332,#22333,#22334,#22335,#22336,#22337,
#22338,#22339,#22340,#22341,#22342,#22343,#22344,#22345,#22346,#22347,#22348,
#22349,#22350,#22351,#22352,#22353,#22354,#22355,#22356,#22357,#22358,#22359,
#22360,#22361,#22362,#22363,#22364,#22365,#22366,#22367,#22368,#22369,#22370,
#22371,#22372,#22373,#22374,#22375,#22376,#22377),.UNSPECIFIED.,.F.,.F.)
B_SPLINE_CURVE_WITH_KNOTS((6,1,1,1,1,1,1,1,1,1,1,1,1,1,1,1,1,1,1,1,1,1,
1,1,1,1,1,1,1,1,1,1,1,1,1,1,1,1,1,1,1,1,1,1,1,1,1,1,1,1,1,1,1,1,1,1,1,1,
1,1,1,1,1,1,1,6),(0.,0.0153846153846154,0.0307692307692308,0.0461538461538462,
0.0615384615384615,0.0769230769230769,0.0923076923076923,0.107692307692308,
0.123076923076923,0.138461538461538,0.153846153846154,0.169230769230769,
0.184615384615385,0.2,0.215384615384615,0.230769230769231,0.246153846153846,
0.261538461538462,0.276923076923077,0.292307692307692,0.307692307692308,
0.323076923076923,0.338461538461538,0.353846153846154,0.369230769230769,
0.384615384615385,0.4,0.415384615384615,0.430769230769231,0.446153846153846,
0.461538461538462,0.476923076923077,0.492307692307692,0.507692307692308,
0.523076923076923,0.538461538461538,0.553846153846154,0.569230769230769,
0.584615384615384,0.6,0.615384615384615,0.63076923076923,0.646153846153846,
0.661538461538461,0.676923076923076,0.692307692307692,0.707692307692307,
0.723076923076922,0.738461538461538,0.753846153846153,0.769230769230768,
0.784615384615384,0.799999999999999,0.815384615384614,0.83076923076923,
0.846153846153845,0.86153846153846,0.876923076923076,0.892307692307691,
0.907692307692306,0.923076923076922,0.938461538461537,0.953846153846152,
0.969230769230768,0.984615384615383,1.),.UNSPECIFIED.)
CURVE()
GEOMETRIC_REPRESENTATION_ITEM()
RATIONAL_B_SPLINE_CURVE((1.,1.,1.,1.,1.,1.,1.,1.,1.,1.,1.,1.,1.,1.,1.,1.,
1.,1.,1.,1.,1.,1.,1.,1.,1.,1.,1.,1.,1.,1.,1.,1.,1.,1.,1.,1.,1.,1.,1.,1.,
1.,1.,1.,1.,1.,1.,1.,1.,1.,1.,1.,1.,1.,1.,1.,1.,1.,1.,1.,1.,1.,1.,1.,1.,
1.,1.,1.,1.,1.,1.))
REPRESENTATION_ITEM('')
);
#72=(
BOUNDED_CURVE()
B_SPLINE_CURVE(5,(#22381,#22382,#22383,#22384,#22385,#22386,#22387,#22388,
#22389,#22390,#22391,#22392,#22393,#22394,#22395,#22396,#22397,#22398,#22399,
#22400,#22401,#22402,#22403,#22404,#22405,#22406,#22407,#22408,#22409,#22410,
#22411,#22412,#22413,#22414,#22415,#22416,#22417,#22418,#22419,#22420,#22421,
#22422,#22423,#22424,#22425,#22426,#22427,#22428,#22429,#22430,#22431,#22432,
#22433,#22434,#22435,#22436,#22437,#22438,#22439,#22440,#22441,#22442,#22443,
#22444,#22445,#22446,#22447,#22448,#22449,#22450),.UNSPECIFIED.,.F.,.F.)
B_SPLINE_CURVE_WITH_KNOTS((6,1,1,1,1,1,1,1,1,1,1,1,1,1,1,1,1,1,1,1,1,1,
1,1,1,1,1,1,1,1,1,1,1,1,1,1,1,1,1,1,1,1,1,1,1,1,1,1,1,1,1,1,1,1,1,1,1,1,
1,1,1,1,1,1,1,6),(0.,0.0153846153846154,0.0307692307692308,0.0461538461538462,
0.0615384615384615,0.0769230769230769,0.0923076923076923,0.107692307692308,
0.123076923076923,0.138461538461538,0.153846153846154,0.169230769230769,
0.184615384615385,0.2,0.215384615384615,0.230769230769231,0.246153846153846,
0.261538461538462,0.276923076923077,0.292307692307692,0.307692307692308,
0.323076923076923,0.338461538461538,0.353846153846154,0.369230769230769,
0.384615384615385,0.4,0.415384615384615,0.430769230769231,0.446153846153846,
0.461538461538462,0.476923076923077,0.492307692307692,0.507692307692308,
0.523076923076923,0.538461538461538,0.553846153846154,0.569230769230769,
0.584615384615384,0.6,0.615384615384615,0.63076923076923,0.646153846153846,
0.661538461538461,0.676923076923076,0.692307692307692,0.707692307692307,
0.723076923076922,0.738461538461538,0.753846153846153,0.769230769230768,
0.784615384615384,0.799999999999999,0.815384615384614,0.83076923076923,
0.846153846153845,0.86153846153846,0.876923076923076,0.892307692307691,
0.907692307692306,0.923076923076922,0.938461538461537,0.953846153846152,
0.969230769230768,0.984615384615383,1.),.UNSPECIFIED.)
CURVE()
GEOMETRIC_REPRESENTATION_ITEM()
RATIONAL_B_SPLINE_CURVE((1.,1.,1.,1.,1.,1.,1.,1.,1.,1.,1.,1.,1.,1.,1.,1.,
1.,1.,1.,1.,1.,1.,1.,1.,1.,1.,1.,1.,1.,1.,1.,1.,1.,1.,1.,1.,1.,1.,1.,1.,
1.,1.,1.,1.,1.,1.,1.,1.,1.,1.,1.,1.,1.,1.,1.,1.,1.,1.,1.,1.,1.,1.,1.,1.,
1.,1.,1.,1.,1.,1.))
REPRESENTATION_ITEM('')
);
#73=(
BOUNDED_CURVE()
B_SPLINE_CURVE(5,(#22454,#22455,#22456,#22457,#22458,#22459,#22460,#22461,
#22462,#22463,#22464,#22465,#22466,#22467,#22468,#22469,#22470,#22471,#22472,
#22473,#22474,#22475,#22476,#22477,#22478,#22479,#22480,#22481,#22482,#22483,
#22484,#22485,#22486,#22487,#22488,#22489,#22490,#22491,#22492,#22493,#22494,
#22495,#22496,#22497,#22498,#22499,#22500,#22501,#22502,#22503,#22504,#22505,
#22506,#22507,#22508,#22509,#22510,#22511,#22512,#22513,#22514,#22515,#22516,
#22517,#22518,#22519,#22520,#22521,#22522,#22523),.UNSPECIFIED.,.F.,.F.)
B_SPLINE_CURVE_WITH_KNOTS((6,1,1,1,1,1,1,1,1,1,1,1,1,1,1,1,1,1,1,1,1,1,
1,1,1,1,1,1,1,1,1,1,1,1,1,1,1,1,1,1,1,1,1,1,1,1,1,1,1,1,1,1,1,1,1,1,1,1,
1,1,1,1,1,1,1,6),(0.,0.0153846153846154,0.0307692307692308,0.0461538461538462,
0.0615384615384615,0.0769230769230769,0.0923076923076923,0.107692307692308,
0.123076923076923,0.138461538461538,0.153846153846154,0.169230769230769,
0.184615384615385,0.2,0.215384615384615,0.230769230769231,0.246153846153846,
0.261538461538462,0.276923076923077,0.292307692307692,0.307692307692308,
0.323076923076923,0.338461538461538,0.353846153846154,0.369230769230769,
0.384615384615385,0.4,0.415384615384615,0.430769230769231,0.446153846153846,
0.461538461538462,0.476923076923077,0.492307692307692,0.507692307692308,
0.523076923076923,0.538461538461538,0.553846153846154,0.569230769230769,
0.584615384615384,0.6,0.615384615384615,0.63076923076923,0.646153846153846,
0.661538461538461,0.676923076923076,0.692307692307692,0.707692307692307,
0.723076923076922,0.738461538461538,0.753846153846153,0.769230769230768,
0.784615384615384,0.799999999999999,0.815384615384614,0.83076923076923,
0.846153846153845,0.86153846153846,0.876923076923076,0.892307692307691,
0.907692307692306,0.923076923076922,0.938461538461537,0.953846153846152,
0.969230769230768,0.984615384615383,1.),.UNSPECIFIED.)
CURVE()
GEOMETRIC_REPRESENTATION_ITEM()
RATIONAL_B_SPLINE_CURVE((1.,1.,1.,1.,1.,1.,1.,1.,1.,1.,1.,1.,1.,1.,1.,1.,
1.,1.,1.,1.,1.,1.,1.,1.,1.,1.,1.,1.,1.,1.,1.,1.,1.,1.,1.,1.,1.,1.,1.,1.,
1.,1.,1.,1.,1.,1.,1.,1.,1.,1.,1.,1.,1.,1.,1.,1.,1.,1.,1.,1.,1.,1.,1.,1.,
1.,1.,1.,1.,1.,1.))
REPRESENTATION_ITEM('')
);
#74=(
BOUNDED_CURVE()
B_SPLINE_CURVE(5,(#22527,#22528,#22529,#22530,#22531,#22532,#22533,#22534,
#22535,#22536,#22537,#22538,#22539,#22540,#22541,#22542,#22543,#22544,#22545,
#22546,#22547,#22548,#22549,#22550,#22551,#22552,#22553,#22554,#22555,#22556,
#22557,#22558,#22559,#22560,#22561,#22562,#22563,#22564,#22565,#22566,#22567,
#22568,#22569,#22570,#22571,#22572,#22573,#22574,#22575,#22576,#22577,#22578,
#22579,#22580,#22581,#22582,#22583,#22584,#22585,#22586,#22587,#22588,#22589,
#22590,#22591,#22592,#22593,#22594,#22595,#22596),.UNSPECIFIED.,.F.,.F.)
B_SPLINE_CURVE_WITH_KNOTS((6,1,1,1,1,1,1,1,1,1,1,1,1,1,1,1,1,1,1,1,1,1,
1,1,1,1,1,1,1,1,1,1,1,1,1,1,1,1,1,1,1,1,1,1,1,1,1,1,1,1,1,1,1,1,1,1,1,1,
1,1,1,1,1,1,1,6),(0.,0.0153846153846154,0.0307692307692308,0.0461538461538462,
0.0615384615384615,0.0769230769230769,0.0923076923076923,0.107692307692308,
0.123076923076923,0.138461538461538,0.153846153846154,0.169230769230769,
0.184615384615385,0.2,0.215384615384615,0.230769230769231,0.246153846153846,
0.261538461538462,0.276923076923077,0.292307692307692,0.307692307692308,
0.323076923076923,0.338461538461538,0.353846153846154,0.369230769230769,
0.384615384615385,0.4,0.415384615384615,0.430769230769231,0.446153846153846,
0.461538461538462,0.476923076923077,0.492307692307692,0.507692307692308,
0.523076923076923,0.538461538461538,0.553846153846154,0.569230769230769,
0.584615384615384,0.6,0.615384615384615,0.63076923076923,0.646153846153846,
0.661538461538461,0.676923076923076,0.692307692307692,0.707692307692307,
0.723076923076922,0.738461538461538,0.753846153846153,0.769230769230768,
0.784615384615384,0.799999999999999,0.815384615384614,0.83076923076923,
0.846153846153845,0.86153846153846,0.876923076923076,0.892307692307691,
0.907692307692306,0.923076923076922,0.938461538461537,0.953846153846152,
0.969230769230768,0.984615384615383,1.),.UNSPECIFIED.)
CURVE()
GEOMETRIC_REPRESENTATION_ITEM()
RATIONAL_B_SPLINE_CURVE((1.,1.,1.,1.,1.,1.,1.,1.,1.,1.,1.,1.,1.,1.,1.,1.,
1.,1.,1.,1.,1.,1.,1.,1.,1.,1.,1.,1.,1.,1.,1.,1.,1.,1.,1.,1.,1.,1.,1.,1.,
1.,1.,1.,1.,1.,1.,1.,1.,1.,1.,1.,1.,1.,1.,1.,1.,1.,1.,1.,1.,1.,1.,1.,1.,
1.,1.,1.,1.,1.,1.))
REPRESENTATION_ITEM('')
);
#75=(
BOUNDED_CURVE()
B_SPLINE_CURVE(5,(#22600,#22601,#22602,#22603,#22604,#22605,#22606,#22607,
#22608,#22609,#22610,#22611,#22612,#22613,#22614,#22615,#22616,#22617,#22618,
#22619,#22620,#22621,#22622,#22623,#22624,#22625,#22626,#22627,#22628,#22629,
#22630,#22631,#22632,#22633,#22634,#22635,#22636,#22637,#22638,#22639,#22640,
#22641,#22642,#22643,#22644,#22645,#22646,#22647,#22648,#22649,#22650,#22651,
#22652,#22653,#22654,#22655,#22656,#22657,#22658,#22659,#22660,#22661,#22662,
#22663,#22664,#22665,#22666,#22667,#22668,#22669),.UNSPECIFIED.,.F.,.F.)
B_SPLINE_CURVE_WITH_KNOTS((6,1,1,1,1,1,1,1,1,1,1,1,1,1,1,1,1,1,1,1,1,1,
1,1,1,1,1,1,1,1,1,1,1,1,1,1,1,1,1,1,1,1,1,1,1,1,1,1,1,1,1,1,1,1,1,1,1,1,
1,1,1,1,1,1,1,6),(0.,0.0153846153846154,0.0307692307692308,0.0461538461538462,
0.0615384615384615,0.0769230769230769,0.0923076923076923,0.107692307692308,
0.123076923076923,0.138461538461538,0.153846153846154,0.169230769230769,
0.184615384615385,0.2,0.215384615384615,0.230769230769231,0.246153846153846,
0.261538461538462,0.276923076923077,0.292307692307692,0.307692307692308,
0.323076923076923,0.338461538461538,0.353846153846154,0.369230769230769,
0.384615384615385,0.4,0.415384615384615,0.430769230769231,0.446153846153846,
0.461538461538462,0.476923076923077,0.492307692307692,0.507692307692308,
0.523076923076923,0.538461538461538,0.553846153846154,0.569230769230769,
0.584615384615384,0.6,0.615384615384615,0.63076923076923,0.646153846153846,
0.661538461538461,0.676923076923076,0.692307692307692,0.707692307692307,
0.723076923076922,0.738461538461538,0.753846153846153,0.769230769230768,
0.784615384615384,0.799999999999999,0.815384615384614,0.83076923076923,
0.846153846153845,0.86153846153846,0.876923076923076,0.892307692307691,
0.907692307692306,0.923076923076922,0.938461538461537,0.953846153846152,
0.969230769230768,0.984615384615383,1.),.UNSPECIFIED.)
CURVE()
GEOMETRIC_REPRESENTATION_ITEM()
RATIONAL_B_SPLINE_CURVE((1.,1.,1.,1.,1.,1.,1.,1.,1.,1.,1.,1.,1.,1.,1.,1.,
1.,1.,1.,1.,1.,1.,1.,1.,1.,1.,1.,1.,1.,1.,1.,1.,1.,1.,1.,1.,1.,1.,1.,1.,
1.,1.,1.,1.,1.,1.,1.,1.,1.,1.,1.,1.,1.,1.,1.,1.,1.,1.,1.,1.,1.,1.,1.,1.,
1.,1.,1.,1.,1.,1.))
REPRESENTATION_ITEM('')
);
#76=(
BOUNDED_CURVE()
B_SPLINE_CURVE(5,(#22673,#22674,#22675,#22676,#22677,#22678,#22679,#22680,
#22681,#22682,#22683,#22684,#22685,#22686,#22687,#22688,#22689,#22690,#22691,
#22692,#22693,#22694,#22695,#22696,#22697,#22698,#22699,#22700,#22701,#22702,
#22703,#22704,#22705,#22706,#22707,#22708,#22709,#22710,#22711,#22712,#22713,
#22714,#22715,#22716,#22717,#22718,#22719,#22720,#22721,#22722,#22723,#22724,
#22725,#22726,#22727,#22728,#22729,#22730,#22731,#22732,#22733,#22734,#22735,
#22736,#22737,#22738,#22739,#22740,#22741,#22742),.UNSPECIFIED.,.F.,.F.)
B_SPLINE_CURVE_WITH_KNOTS((6,1,1,1,1,1,1,1,1,1,1,1,1,1,1,1,1,1,1,1,1,1,
1,1,1,1,1,1,1,1,1,1,1,1,1,1,1,1,1,1,1,1,1,1,1,1,1,1,1,1,1,1,1,1,1,1,1,1,
1,1,1,1,1,1,1,6),(0.,0.0153846153846154,0.0307692307692308,0.0461538461538462,
0.0615384615384615,0.0769230769230769,0.0923076923076923,0.107692307692308,
0.123076923076923,0.138461538461538,0.153846153846154,0.169230769230769,
0.184615384615385,0.2,0.215384615384615,0.230769230769231,0.246153846153846,
0.261538461538462,0.276923076923077,0.292307692307692,0.307692307692308,
0.323076923076923,0.338461538461538,0.353846153846154,0.369230769230769,
0.384615384615385,0.4,0.415384615384615,0.430769230769231,0.446153846153846,
0.461538461538462,0.476923076923077,0.492307692307692,0.507692307692308,
0.523076923076923,0.538461538461538,0.553846153846154,0.569230769230769,
0.584615384615384,0.6,0.615384615384615,0.63076923076923,0.646153846153846,
0.661538461538461,0.676923076923076,0.692307692307692,0.707692307692307,
0.723076923076922,0.738461538461538,0.753846153846153,0.769230769230768,
0.784615384615384,0.799999999999999,0.815384615384614,0.83076923076923,
0.846153846153845,0.86153846153846,0.876923076923076,0.892307692307691,
0.907692307692306,0.923076923076922,0.938461538461537,0.953846153846152,
0.969230769230768,0.984615384615383,1.),.UNSPECIFIED.)
CURVE()
GEOMETRIC_REPRESENTATION_ITEM()
RATIONAL_B_SPLINE_CURVE((1.,1.,1.,1.,1.,1.,1.,1.,1.,1.,1.,1.,1.,1.,1.,1.,
1.,1.,1.,1.,1.,1.,1.,1.,1.,1.,1.,1.,1.,1.,1.,1.,1.,1.,1.,1.,1.,1.,1.,1.,
1.,1.,1.,1.,1.,1.,1.,1.,1.,1.,1.,1.,1.,1.,1.,1.,1.,1.,1.,1.,1.,1.,1.,1.,
1.,1.,1.,1.,1.,1.))
REPRESENTATION_ITEM('')
);
#77=(
BOUNDED_CURVE()
B_SPLINE_CURVE(5,(#22746,#22747,#22748,#22749,#22750,#22751,#22752,#22753,
#22754,#22755,#22756,#22757,#22758,#22759,#22760,#22761,#22762,#22763,#22764,
#22765,#22766,#22767,#22768,#22769,#22770,#22771,#22772,#22773,#22774,#22775,
#22776,#22777,#22778,#22779,#22780,#22781,#22782,#22783,#22784,#22785,#22786,
#22787,#22788,#22789,#22790,#22791,#22792,#22793,#22794,#22795,#22796,#22797,
#22798,#22799,#22800,#22801,#22802,#22803,#22804,#22805,#22806,#22807,#22808,
#22809,#22810,#22811,#22812,#22813,#22814,#22815),.UNSPECIFIED.,.F.,.F.)
B_SPLINE_CURVE_WITH_KNOTS((6,1,1,1,1,1,1,1,1,1,1,1,1,1,1,1,1,1,1,1,1,1,
1,1,1,1,1,1,1,1,1,1,1,1,1,1,1,1,1,1,1,1,1,1,1,1,1,1,1,1,1,1,1,1,1,1,1,1,
1,1,1,1,1,1,1,6),(0.,0.0153846153846154,0.0307692307692308,0.0461538461538462,
0.0615384615384615,0.0769230769230769,0.0923076923076923,0.107692307692308,
0.123076923076923,0.138461538461538,0.153846153846154,0.169230769230769,
0.184615384615385,0.2,0.215384615384615,0.230769230769231,0.246153846153846,
0.261538461538462,0.276923076923077,0.292307692307692,0.307692307692308,
0.323076923076923,0.338461538461538,0.353846153846154,0.369230769230769,
0.384615384615385,0.4,0.415384615384615,0.430769230769231,0.446153846153846,
0.461538461538462,0.476923076923077,0.492307692307692,0.507692307692308,
0.523076923076923,0.538461538461538,0.553846153846154,0.569230769230769,
0.584615384615384,0.6,0.615384615384615,0.63076923076923,0.646153846153846,
0.661538461538461,0.676923076923076,0.692307692307692,0.707692307692307,
0.723076923076922,0.738461538461538,0.753846153846153,0.769230769230768,
0.784615384615384,0.799999999999999,0.815384615384614,0.83076923076923,
0.846153846153845,0.86153846153846,0.876923076923076,0.892307692307691,
0.907692307692306,0.923076923076922,0.938461538461537,0.953846153846152,
0.969230769230768,0.984615384615383,1.),.UNSPECIFIED.)
CURVE()
GEOMETRIC_REPRESENTATION_ITEM()
RATIONAL_B_SPLINE_CURVE((1.,1.,1.,1.,1.,1.,1.,1.,1.,1.,1.,1.,1.,1.,1.,1.,
1.,1.,1.,1.,1.,1.,1.,1.,1.,1.,1.,1.,1.,1.,1.,1.,1.,1.,1.,1.,1.,1.,1.,1.,
1.,1.,1.,1.,1.,1.,1.,1.,1.,1.,1.,1.,1.,1.,1.,1.,1.,1.,1.,1.,1.,1.,1.,1.,
1.,1.,1.,1.,1.,1.))
REPRESENTATION_ITEM('')
);
#78=(
BOUNDED_CURVE()
B_SPLINE_CURVE(5,(#22819,#22820,#22821,#22822,#22823,#22824,#22825,#22826,
#22827,#22828,#22829,#22830,#22831,#22832,#22833,#22834,#22835,#22836,#22837,
#22838,#22839,#22840,#22841,#22842,#22843,#22844,#22845,#22846,#22847,#22848,
#22849,#22850,#22851,#22852,#22853,#22854,#22855,#22856,#22857,#22858,#22859,
#22860,#22861,#22862,#22863,#22864,#22865,#22866,#22867,#22868,#22869,#22870,
#22871,#22872,#22873,#22874,#22875,#22876,#22877,#22878,#22879,#22880,#22881,
#22882,#22883,#22884,#22885,#22886,#22887,#22888),.UNSPECIFIED.,.F.,.F.)
B_SPLINE_CURVE_WITH_KNOTS((6,1,1,1,1,1,1,1,1,1,1,1,1,1,1,1,1,1,1,1,1,1,
1,1,1,1,1,1,1,1,1,1,1,1,1,1,1,1,1,1,1,1,1,1,1,1,1,1,1,1,1,1,1,1,1,1,1,1,
1,1,1,1,1,1,1,6),(0.,0.0153846153846154,0.0307692307692308,0.0461538461538462,
0.0615384615384615,0.0769230769230769,0.0923076923076923,0.107692307692308,
0.123076923076923,0.138461538461538,0.153846153846154,0.169230769230769,
0.184615384615385,0.2,0.215384615384615,0.230769230769231,0.246153846153846,
0.261538461538462,0.276923076923077,0.292307692307692,0.307692307692308,
0.323076923076923,0.338461538461538,0.353846153846154,0.369230769230769,
0.384615384615385,0.4,0.415384615384615,0.430769230769231,0.446153846153846,
0.461538461538462,0.476923076923077,0.492307692307692,0.507692307692308,
0.523076923076923,0.538461538461538,0.553846153846154,0.569230769230769,
0.584615384615384,0.6,0.615384615384615,0.63076923076923,0.646153846153846,
0.661538461538461,0.676923076923076,0.692307692307692,0.707692307692307,
0.723076923076922,0.738461538461538,0.753846153846153,0.769230769230768,
0.784615384615384,0.799999999999999,0.815384615384614,0.83076923076923,
0.846153846153845,0.86153846153846,0.876923076923076,0.892307692307691,
0.907692307692306,0.923076923076922,0.938461538461537,0.953846153846152,
0.969230769230768,0.984615384615383,1.),.UNSPECIFIED.)
CURVE()
GEOMETRIC_REPRESENTATION_ITEM()
RATIONAL_B_SPLINE_CURVE((1.,1.,1.,1.,1.,1.,1.,1.,1.,1.,1.,1.,1.,1.,1.,1.,
1.,1.,1.,1.,1.,1.,1.,1.,1.,1.,1.,1.,1.,1.,1.,1.,1.,1.,1.,1.,1.,1.,1.,1.,
1.,1.,1.,1.,1.,1.,1.,1.,1.,1.,1.,1.,1.,1.,1.,1.,1.,1.,1.,1.,1.,1.,1.,1.,
1.,1.,1.,1.,1.,1.))
REPRESENTATION_ITEM('')
);
#79=(
BOUNDED_CURVE()
B_SPLINE_CURVE(5,(#22892,#22893,#22894,#22895,#22896,#22897,#22898,#22899,
#22900,#22901,#22902,#22903,#22904,#22905,#22906,#22907,#22908,#22909,#22910,
#22911,#22912,#22913,#22914,#22915,#22916,#22917,#22918,#22919,#22920,#22921,
#22922,#22923,#22924,#22925,#22926,#22927,#22928,#22929,#22930,#22931,#22932,
#22933,#22934,#22935,#22936,#22937,#22938,#22939,#22940,#22941,#22942,#22943,
#22944,#22945,#22946,#22947,#22948,#22949,#22950,#22951,#22952,#22953,#22954,
#22955,#22956,#22957,#22958,#22959,#22960,#22961),.UNSPECIFIED.,.F.,.F.)
B_SPLINE_CURVE_WITH_KNOTS((6,1,1,1,1,1,1,1,1,1,1,1,1,1,1,1,1,1,1,1,1,1,
1,1,1,1,1,1,1,1,1,1,1,1,1,1,1,1,1,1,1,1,1,1,1,1,1,1,1,1,1,1,1,1,1,1,1,1,
1,1,1,1,1,1,1,6),(0.,0.0153846153846154,0.0307692307692308,0.0461538461538462,
0.0615384615384615,0.0769230769230769,0.0923076923076923,0.107692307692308,
0.123076923076923,0.138461538461538,0.153846153846154,0.169230769230769,
0.184615384615385,0.2,0.215384615384615,0.230769230769231,0.246153846153846,
0.261538461538462,0.276923076923077,0.292307692307692,0.307692307692308,
0.323076923076923,0.338461538461538,0.353846153846154,0.369230769230769,
0.384615384615385,0.4,0.415384615384615,0.430769230769231,0.446153846153846,
0.461538461538462,0.476923076923077,0.492307692307692,0.507692307692308,
0.523076923076923,0.538461538461538,0.553846153846154,0.569230769230769,
0.584615384615384,0.6,0.615384615384615,0.63076923076923,0.646153846153846,
0.661538461538461,0.676923076923076,0.692307692307692,0.707692307692307,
0.723076923076922,0.738461538461538,0.753846153846153,0.769230769230768,
0.784615384615384,0.799999999999999,0.815384615384614,0.83076923076923,
0.846153846153845,0.86153846153846,0.876923076923076,0.892307692307691,
0.907692307692306,0.923076923076922,0.938461538461537,0.953846153846152,
0.969230769230768,0.984615384615383,1.),.UNSPECIFIED.)
CURVE()
GEOMETRIC_REPRESENTATION_ITEM()
RATIONAL_B_SPLINE_CURVE((1.,1.,1.,1.,1.,1.,1.,1.,1.,1.,1.,1.,1.,1.,1.,1.,
1.,1.,1.,1.,1.,1.,1.,1.,1.,1.,1.,1.,1.,1.,1.,1.,1.,1.,1.,1.,1.,1.,1.,1.,
1.,1.,1.,1.,1.,1.,1.,1.,1.,1.,1.,1.,1.,1.,1.,1.,1.,1.,1.,1.,1.,1.,1.,1.,
1.,1.,1.,1.,1.,1.))
REPRESENTATION_ITEM('')
);
#80=(
BOUNDED_CURVE()
B_SPLINE_CURVE(5,(#22965,#22966,#22967,#22968,#22969,#22970,#22971,#22972,
#22973,#22974,#22975,#22976,#22977,#22978,#22979,#22980,#22981,#22982,#22983,
#22984,#22985,#22986,#22987,#22988,#22989,#22990,#22991,#22992,#22993,#22994,
#22995,#22996,#22997,#22998,#22999,#23000,#23001,#23002,#23003,#23004,#23005,
#23006,#23007,#23008,#23009,#23010,#23011,#23012,#23013,#23014,#23015,#23016,
#23017,#23018,#23019,#23020,#23021,#23022,#23023,#23024,#23025,#23026,#23027,
#23028,#23029,#23030,#23031,#23032,#23033,#23034),.UNSPECIFIED.,.F.,.F.)
B_SPLINE_CURVE_WITH_KNOTS((6,1,1,1,1,1,1,1,1,1,1,1,1,1,1,1,1,1,1,1,1,1,
1,1,1,1,1,1,1,1,1,1,1,1,1,1,1,1,1,1,1,1,1,1,1,1,1,1,1,1,1,1,1,1,1,1,1,1,
1,1,1,1,1,1,1,6),(0.,0.0153846153846154,0.0307692307692308,0.0461538461538462,
0.0615384615384615,0.0769230769230769,0.0923076923076923,0.107692307692308,
0.123076923076923,0.138461538461538,0.153846153846154,0.169230769230769,
0.184615384615385,0.2,0.215384615384615,0.230769230769231,0.246153846153846,
0.261538461538462,0.276923076923077,0.292307692307692,0.307692307692308,
0.323076923076923,0.338461538461538,0.353846153846154,0.369230769230769,
0.384615384615385,0.4,0.415384615384615,0.430769230769231,0.446153846153846,
0.461538461538462,0.476923076923077,0.492307692307692,0.507692307692308,
0.523076923076923,0.538461538461538,0.553846153846154,0.569230769230769,
0.584615384615384,0.6,0.615384615384615,0.63076923076923,0.646153846153846,
0.661538461538461,0.676923076923076,0.692307692307692,0.707692307692307,
0.723076923076922,0.738461538461538,0.753846153846153,0.769230769230768,
0.784615384615384,0.799999999999999,0.815384615384614,0.83076923076923,
0.846153846153845,0.86153846153846,0.876923076923076,0.892307692307691,
0.907692307692306,0.923076923076922,0.938461538461537,0.953846153846152,
0.969230769230768,0.984615384615383,1.),.UNSPECIFIED.)
CURVE()
GEOMETRIC_REPRESENTATION_ITEM()
RATIONAL_B_SPLINE_CURVE((1.,1.,1.,1.,1.,1.,1.,1.,1.,1.,1.,1.,1.,1.,1.,1.,
1.,1.,1.,1.,1.,1.,1.,1.,1.,1.,1.,1.,1.,1.,1.,1.,1.,1.,1.,1.,1.,1.,1.,1.,
1.,1.,1.,1.,1.,1.,1.,1.,1.,1.,1.,1.,1.,1.,1.,1.,1.,1.,1.,1.,1.,1.,1.,1.,
1.,1.,1.,1.,1.,1.))
REPRESENTATION_ITEM('')
);
#81=(
BOUNDED_CURVE()
B_SPLINE_CURVE(5,(#23038,#23039,#23040,#23041,#23042,#23043,#23044,#23045,
#23046,#23047,#23048,#23049,#23050,#23051,#23052,#23053,#23054,#23055,#23056,
#23057,#23058,#23059,#23060,#23061,#23062,#23063,#23064,#23065,#23066,#23067,
#23068,#23069,#23070,#23071,#23072,#23073,#23074,#23075,#23076,#23077,#23078,
#23079,#23080,#23081,#23082,#23083,#23084,#23085,#23086,#23087,#23088,#23089,
#23090,#23091,#23092,#23093,#23094,#23095,#23096,#23097,#23098,#23099,#23100,
#23101,#23102,#23103,#23104,#23105,#23106,#23107),.UNSPECIFIED.,.F.,.F.)
B_SPLINE_CURVE_WITH_KNOTS((6,1,1,1,1,1,1,1,1,1,1,1,1,1,1,1,1,1,1,1,1,1,
1,1,1,1,1,1,1,1,1,1,1,1,1,1,1,1,1,1,1,1,1,1,1,1,1,1,1,1,1,1,1,1,1,1,1,1,
1,1,1,1,1,1,1,6),(0.,0.0153846153846154,0.0307692307692308,0.0461538461538462,
0.0615384615384615,0.0769230769230769,0.0923076923076923,0.107692307692308,
0.123076923076923,0.138461538461538,0.153846153846154,0.169230769230769,
0.184615384615385,0.2,0.215384615384615,0.230769230769231,0.246153846153846,
0.261538461538462,0.276923076923077,0.292307692307692,0.307692307692308,
0.323076923076923,0.338461538461538,0.353846153846154,0.369230769230769,
0.384615384615385,0.4,0.415384615384615,0.430769230769231,0.446153846153846,
0.461538461538462,0.476923076923077,0.492307692307692,0.507692307692308,
0.523076923076923,0.538461538461538,0.553846153846154,0.569230769230769,
0.584615384615384,0.6,0.615384615384615,0.63076923076923,0.646153846153846,
0.661538461538461,0.676923076923076,0.692307692307692,0.707692307692307,
0.723076923076922,0.738461538461538,0.753846153846153,0.769230769230768,
0.784615384615384,0.799999999999999,0.815384615384614,0.83076923076923,
0.846153846153845,0.86153846153846,0.876923076923076,0.892307692307691,
0.907692307692306,0.923076923076922,0.938461538461537,0.953846153846152,
0.969230769230768,0.984615384615383,1.),.UNSPECIFIED.)
CURVE()
GEOMETRIC_REPRESENTATION_ITEM()
RATIONAL_B_SPLINE_CURVE((1.,1.,1.,1.,1.,1.,1.,1.,1.,1.,1.,1.,1.,1.,1.,1.,
1.,1.,1.,1.,1.,1.,1.,1.,1.,1.,1.,1.,1.,1.,1.,1.,1.,1.,1.,1.,1.,1.,1.,1.,
1.,1.,1.,1.,1.,1.,1.,1.,1.,1.,1.,1.,1.,1.,1.,1.,1.,1.,1.,1.,1.,1.,1.,1.,
1.,1.,1.,1.,1.,1.))
REPRESENTATION_ITEM('')
);
#82=(
BOUNDED_CURVE()
B_SPLINE_CURVE(5,(#23111,#23112,#23113,#23114,#23115,#23116,#23117,#23118,
#23119,#23120,#23121,#23122,#23123,#23124,#23125,#23126,#23127,#23128,#23129,
#23130,#23131,#23132,#23133,#23134,#23135,#23136,#23137,#23138,#23139,#23140,
#23141,#23142,#23143,#23144,#23145,#23146,#23147,#23148,#23149,#23150,#23151,
#23152,#23153,#23154,#23155,#23156,#23157,#23158,#23159,#23160,#23161,#23162,
#23163,#23164,#23165,#23166,#23167,#23168,#23169,#23170,#23171,#23172,#23173,
#23174,#23175,#23176,#23177,#23178,#23179,#23180),.UNSPECIFIED.,.F.,.F.)
B_SPLINE_CURVE_WITH_KNOTS((6,1,1,1,1,1,1,1,1,1,1,1,1,1,1,1,1,1,1,1,1,1,
1,1,1,1,1,1,1,1,1,1,1,1,1,1,1,1,1,1,1,1,1,1,1,1,1,1,1,1,1,1,1,1,1,1,1,1,
1,1,1,1,1,1,1,6),(0.,0.0153846153846154,0.0307692307692308,0.0461538461538462,
0.0615384615384615,0.0769230769230769,0.0923076923076923,0.107692307692308,
0.123076923076923,0.138461538461538,0.153846153846154,0.169230769230769,
0.184615384615385,0.2,0.215384615384615,0.230769230769231,0.246153846153846,
0.261538461538462,0.276923076923077,0.292307692307692,0.307692307692308,
0.323076923076923,0.338461538461538,0.353846153846154,0.369230769230769,
0.384615384615385,0.4,0.415384615384615,0.430769230769231,0.446153846153846,
0.461538461538462,0.476923076923077,0.492307692307692,0.507692307692308,
0.523076923076923,0.538461538461538,0.553846153846154,0.569230769230769,
0.584615384615384,0.6,0.615384615384615,0.63076923076923,0.646153846153846,
0.661538461538461,0.676923076923076,0.692307692307692,0.707692307692307,
0.723076923076922,0.738461538461538,0.753846153846153,0.769230769230768,
0.784615384615384,0.799999999999999,0.815384615384614,0.83076923076923,
0.846153846153845,0.86153846153846,0.876923076923076,0.892307692307691,
0.907692307692306,0.923076923076922,0.938461538461537,0.953846153846152,
0.969230769230768,0.984615384615383,1.),.UNSPECIFIED.)
CURVE()
GEOMETRIC_REPRESENTATION_ITEM()
RATIONAL_B_SPLINE_CURVE((1.,1.,1.,1.,1.,1.,1.,1.,1.,1.,1.,1.,1.,1.,1.,1.,
1.,1.,1.,1.,1.,1.,1.,1.,1.,1.,1.,1.,1.,1.,1.,1.,1.,1.,1.,1.,1.,1.,1.,1.,
1.,1.,1.,1.,1.,1.,1.,1.,1.,1.,1.,1.,1.,1.,1.,1.,1.,1.,1.,1.,1.,1.,1.,1.,
1.,1.,1.,1.,1.,1.))
REPRESENTATION_ITEM('')
);
#83=(
BOUNDED_CURVE()
B_SPLINE_CURVE(5,(#23184,#23185,#23186,#23187,#23188,#23189,#23190,#23191,
#23192,#23193,#23194,#23195,#23196,#23197,#23198,#23199,#23200,#23201,#23202,
#23203,#23204,#23205,#23206,#23207,#23208,#23209,#23210,#23211,#23212,#23213,
#23214,#23215,#23216,#23217,#23218,#23219,#23220,#23221,#23222,#23223,#23224,
#23225,#23226,#23227,#23228,#23229,#23230,#23231,#23232,#23233,#23234,#23235,
#23236,#23237,#23238,#23239,#23240,#23241,#23242,#23243,#23244,#23245,#23246,
#23247,#23248,#23249,#23250,#23251,#23252,#23253),.UNSPECIFIED.,.F.,.F.)
B_SPLINE_CURVE_WITH_KNOTS((6,1,1,1,1,1,1,1,1,1,1,1,1,1,1,1,1,1,1,1,1,1,
1,1,1,1,1,1,1,1,1,1,1,1,1,1,1,1,1,1,1,1,1,1,1,1,1,1,1,1,1,1,1,1,1,1,1,1,
1,1,1,1,1,1,1,6),(0.,0.0153846153846154,0.0307692307692308,0.0461538461538462,
0.0615384615384615,0.0769230769230769,0.0923076923076923,0.107692307692308,
0.123076923076923,0.138461538461538,0.153846153846154,0.169230769230769,
0.184615384615385,0.2,0.215384615384615,0.230769230769231,0.246153846153846,
0.261538461538462,0.276923076923077,0.292307692307692,0.307692307692308,
0.323076923076923,0.338461538461538,0.353846153846154,0.369230769230769,
0.384615384615385,0.4,0.415384615384615,0.430769230769231,0.446153846153846,
0.461538461538462,0.476923076923077,0.492307692307692,0.507692307692308,
0.523076923076923,0.538461538461538,0.553846153846154,0.569230769230769,
0.584615384615384,0.6,0.615384615384615,0.63076923076923,0.646153846153846,
0.661538461538461,0.676923076923076,0.692307692307692,0.707692307692307,
0.723076923076922,0.738461538461538,0.753846153846153,0.769230769230768,
0.784615384615384,0.799999999999999,0.815384615384614,0.83076923076923,
0.846153846153845,0.86153846153846,0.876923076923076,0.892307692307691,
0.907692307692306,0.923076923076922,0.938461538461537,0.953846153846152,
0.969230769230768,0.984615384615383,1.),.UNSPECIFIED.)
CURVE()
GEOMETRIC_REPRESENTATION_ITEM()
RATIONAL_B_SPLINE_CURVE((1.,1.,1.,1.,1.,1.,1.,1.,1.,1.,1.,1.,1.,1.,1.,1.,
1.,1.,1.,1.,1.,1.,1.,1.,1.,1.,1.,1.,1.,1.,1.,1.,1.,1.,1.,1.,1.,1.,1.,1.,
1.,1.,1.,1.,1.,1.,1.,1.,1.,1.,1.,1.,1.,1.,1.,1.,1.,1.,1.,1.,1.,1.,1.,1.,
1.,1.,1.,1.,1.,1.))
REPRESENTATION_ITEM('')
);
#84=(
BOUNDED_CURVE()
B_SPLINE_CURVE(5,(#23257,#23258,#23259,#23260,#23261,#23262,#23263,#23264,
#23265,#23266,#23267,#23268,#23269,#23270,#23271,#23272,#23273,#23274,#23275,
#23276,#23277,#23278,#23279,#23280,#23281,#23282,#23283,#23284,#23285,#23286,
#23287,#23288,#23289,#23290,#23291,#23292,#23293,#23294,#23295,#23296,#23297,
#23298,#23299,#23300,#23301,#23302,#23303,#23304,#23305,#23306,#23307,#23308,
#23309,#23310,#23311,#23312,#23313,#23314,#23315,#23316,#23317,#23318,#23319,
#23320,#23321,#23322,#23323,#23324,#23325,#23326),.UNSPECIFIED.,.F.,.F.)
B_SPLINE_CURVE_WITH_KNOTS((6,1,1,1,1,1,1,1,1,1,1,1,1,1,1,1,1,1,1,1,1,1,
1,1,1,1,1,1,1,1,1,1,1,1,1,1,1,1,1,1,1,1,1,1,1,1,1,1,1,1,1,1,1,1,1,1,1,1,
1,1,1,1,1,1,1,6),(0.,0.0153846153846154,0.0307692307692308,0.0461538461538462,
0.0615384615384615,0.0769230769230769,0.0923076923076923,0.107692307692308,
0.123076923076923,0.138461538461538,0.153846153846154,0.169230769230769,
0.184615384615385,0.2,0.215384615384615,0.230769230769231,0.246153846153846,
0.261538461538462,0.276923076923077,0.292307692307692,0.307692307692308,
0.323076923076923,0.338461538461538,0.353846153846154,0.369230769230769,
0.384615384615385,0.4,0.415384615384615,0.430769230769231,0.446153846153846,
0.461538461538462,0.476923076923077,0.492307692307692,0.507692307692308,
0.523076923076923,0.538461538461538,0.553846153846154,0.569230769230769,
0.584615384615384,0.6,0.615384615384615,0.63076923076923,0.646153846153846,
0.661538461538461,0.676923076923076,0.692307692307692,0.707692307692307,
0.723076923076922,0.738461538461538,0.753846153846153,0.769230769230768,
0.784615384615384,0.799999999999999,0.815384615384614,0.83076923076923,
0.846153846153845,0.86153846153846,0.876923076923076,0.892307692307691,
0.907692307692306,0.923076923076922,0.938461538461537,0.953846153846152,
0.969230769230768,0.984615384615383,1.),.UNSPECIFIED.)
CURVE()
GEOMETRIC_REPRESENTATION_ITEM()
RATIONAL_B_SPLINE_CURVE((1.,1.,1.,1.,1.,1.,1.,1.,1.,1.,1.,1.,1.,1.,1.,1.,
1.,1.,1.,1.,1.,1.,1.,1.,1.,1.,1.,1.,1.,1.,1.,1.,1.,1.,1.,1.,1.,1.,1.,1.,
1.,1.,1.,1.,1.,1.,1.,1.,1.,1.,1.,1.,1.,1.,1.,1.,1.,1.,1.,1.,1.,1.,1.,1.,
1.,1.,1.,1.,1.,1.))
REPRESENTATION_ITEM('')
);
#85=(
BOUNDED_CURVE()
B_SPLINE_CURVE(5,(#23330,#23331,#23332,#23333,#23334,#23335,#23336,#23337,
#23338,#23339,#23340,#23341,#23342,#23343,#23344,#23345,#23346,#23347,#23348,
#23349,#23350,#23351,#23352,#23353,#23354,#23355,#23356,#23357,#23358,#23359,
#23360,#23361,#23362,#23363,#23364,#23365,#23366,#23367,#23368,#23369,#23370,
#23371,#23372,#23373,#23374,#23375,#23376,#23377,#23378,#23379,#23380,#23381,
#23382,#23383,#23384,#23385,#23386,#23387,#23388,#23389,#23390,#23391,#23392,
#23393,#23394,#23395,#23396,#23397,#23398,#23399),.UNSPECIFIED.,.F.,.F.)
B_SPLINE_CURVE_WITH_KNOTS((6,1,1,1,1,1,1,1,1,1,1,1,1,1,1,1,1,1,1,1,1,1,
1,1,1,1,1,1,1,1,1,1,1,1,1,1,1,1,1,1,1,1,1,1,1,1,1,1,1,1,1,1,1,1,1,1,1,1,
1,1,1,1,1,1,1,6),(0.,0.0153846153846154,0.0307692307692308,0.0461538461538462,
0.0615384615384615,0.0769230769230769,0.0923076923076923,0.107692307692308,
0.123076923076923,0.138461538461538,0.153846153846154,0.169230769230769,
0.184615384615385,0.2,0.215384615384615,0.230769230769231,0.246153846153846,
0.261538461538462,0.276923076923077,0.292307692307692,0.307692307692308,
0.323076923076923,0.338461538461538,0.353846153846154,0.369230769230769,
0.384615384615385,0.4,0.415384615384615,0.430769230769231,0.446153846153846,
0.461538461538462,0.476923076923077,0.492307692307692,0.507692307692308,
0.523076923076923,0.538461538461538,0.553846153846154,0.569230769230769,
0.584615384615384,0.6,0.615384615384615,0.63076923076923,0.646153846153846,
0.661538461538461,0.676923076923076,0.692307692307692,0.707692307692307,
0.723076923076922,0.738461538461538,0.753846153846153,0.769230769230768,
0.784615384615384,0.799999999999999,0.815384615384614,0.83076923076923,
0.846153846153845,0.86153846153846,0.876923076923076,0.892307692307691,
0.907692307692306,0.923076923076922,0.938461538461537,0.953846153846152,
0.969230769230768,0.984615384615383,1.),.UNSPECIFIED.)
CURVE()
GEOMETRIC_REPRESENTATION_ITEM()
RATIONAL_B_SPLINE_CURVE((1.,1.,1.,1.,1.,1.,1.,1.,1.,1.,1.,1.,1.,1.,1.,1.,
1.,1.,1.,1.,1.,1.,1.,1.,1.,1.,1.,1.,1.,1.,1.,1.,1.,1.,1.,1.,1.,1.,1.,1.,
1.,1.,1.,1.,1.,1.,1.,1.,1.,1.,1.,1.,1.,1.,1.,1.,1.,1.,1.,1.,1.,1.,1.,1.,
1.,1.,1.,1.,1.,1.))
REPRESENTATION_ITEM('')
);
#86=(
BOUNDED_CURVE()
B_SPLINE_CURVE(5,(#23403,#23404,#23405,#23406,#23407,#23408,#23409,#23410,
#23411,#23412,#23413,#23414,#23415,#23416,#23417,#23418,#23419,#23420,#23421,
#23422,#23423,#23424,#23425,#23426,#23427,#23428,#23429,#23430,#23431,#23432,
#23433,#23434,#23435,#23436,#23437,#23438,#23439,#23440,#23441,#23442,#23443,
#23444,#23445,#23446,#23447,#23448,#23449,#23450,#23451,#23452,#23453,#23454,
#23455,#23456,#23457,#23458,#23459,#23460,#23461,#23462,#23463,#23464,#23465,
#23466,#23467,#23468,#23469,#23470,#23471,#23472),.UNSPECIFIED.,.F.,.F.)
B_SPLINE_CURVE_WITH_KNOTS((6,1,1,1,1,1,1,1,1,1,1,1,1,1,1,1,1,1,1,1,1,1,
1,1,1,1,1,1,1,1,1,1,1,1,1,1,1,1,1,1,1,1,1,1,1,1,1,1,1,1,1,1,1,1,1,1,1,1,
1,1,1,1,1,1,1,6),(0.,0.0153846153846154,0.0307692307692308,0.0461538461538462,
0.0615384615384615,0.0769230769230769,0.0923076923076923,0.107692307692308,
0.123076923076923,0.138461538461538,0.153846153846154,0.169230769230769,
0.184615384615385,0.2,0.215384615384615,0.230769230769231,0.246153846153846,
0.261538461538462,0.276923076923077,0.292307692307692,0.307692307692308,
0.323076923076923,0.338461538461538,0.353846153846154,0.369230769230769,
0.384615384615385,0.4,0.415384615384615,0.430769230769231,0.446153846153846,
0.461538461538462,0.476923076923077,0.492307692307692,0.507692307692308,
0.523076923076923,0.538461538461538,0.553846153846154,0.569230769230769,
0.584615384615384,0.6,0.615384615384615,0.63076923076923,0.646153846153846,
0.661538461538461,0.676923076923076,0.692307692307692,0.707692307692307,
0.723076923076922,0.738461538461538,0.753846153846153,0.769230769230768,
0.784615384615384,0.799999999999999,0.815384615384614,0.83076923076923,
0.846153846153845,0.86153846153846,0.876923076923076,0.892307692307691,
0.907692307692306,0.923076923076922,0.938461538461537,0.953846153846152,
0.969230769230768,0.984615384615383,1.),.UNSPECIFIED.)
CURVE()
GEOMETRIC_REPRESENTATION_ITEM()
RATIONAL_B_SPLINE_CURVE((1.,1.,1.,1.,1.,1.,1.,1.,1.,1.,1.,1.,1.,1.,1.,1.,
1.,1.,1.,1.,1.,1.,1.,1.,1.,1.,1.,1.,1.,1.,1.,1.,1.,1.,1.,1.,1.,1.,1.,1.,
1.,1.,1.,1.,1.,1.,1.,1.,1.,1.,1.,1.,1.,1.,1.,1.,1.,1.,1.,1.,1.,1.,1.,1.,
1.,1.,1.,1.,1.,1.))
REPRESENTATION_ITEM('')
);
#87=(
BOUNDED_CURVE()
B_SPLINE_CURVE(5,(#23476,#23477,#23478,#23479,#23480,#23481,#23482,#23483,
#23484,#23485,#23486,#23487,#23488,#23489,#23490,#23491,#23492,#23493,#23494,
#23495,#23496,#23497,#23498,#23499,#23500,#23501,#23502,#23503,#23504,#23505,
#23506,#23507,#23508,#23509,#23510,#23511,#23512,#23513,#23514,#23515,#23516,
#23517,#23518,#23519,#23520,#23521,#23522,#23523,#23524,#23525,#23526,#23527,
#23528,#23529,#23530,#23531,#23532,#23533,#23534,#23535,#23536,#23537,#23538,
#23539,#23540,#23541,#23542,#23543,#23544,#23545),.UNSPECIFIED.,.F.,.F.)
B_SPLINE_CURVE_WITH_KNOTS((6,1,1,1,1,1,1,1,1,1,1,1,1,1,1,1,1,1,1,1,1,1,
1,1,1,1,1,1,1,1,1,1,1,1,1,1,1,1,1,1,1,1,1,1,1,1,1,1,1,1,1,1,1,1,1,1,1,1,
1,1,1,1,1,1,1,6),(0.,0.0153846153846154,0.0307692307692308,0.0461538461538462,
0.0615384615384615,0.0769230769230769,0.0923076923076923,0.107692307692308,
0.123076923076923,0.138461538461538,0.153846153846154,0.169230769230769,
0.184615384615385,0.2,0.215384615384615,0.230769230769231,0.246153846153846,
0.261538461538462,0.276923076923077,0.292307692307692,0.307692307692308,
0.323076923076923,0.338461538461538,0.353846153846154,0.369230769230769,
0.384615384615385,0.4,0.415384615384615,0.430769230769231,0.446153846153846,
0.461538461538462,0.476923076923077,0.492307692307692,0.507692307692308,
0.523076923076923,0.538461538461538,0.553846153846154,0.569230769230769,
0.584615384615384,0.6,0.615384615384615,0.63076923076923,0.646153846153846,
0.661538461538461,0.676923076923076,0.692307692307692,0.707692307692307,
0.723076923076922,0.738461538461538,0.753846153846153,0.769230769230768,
0.784615384615384,0.799999999999999,0.815384615384614,0.83076923076923,
0.846153846153845,0.86153846153846,0.876923076923076,0.892307692307691,
0.907692307692306,0.923076923076922,0.938461538461537,0.953846153846152,
0.969230769230768,0.984615384615383,1.),.UNSPECIFIED.)
CURVE()
GEOMETRIC_REPRESENTATION_ITEM()
RATIONAL_B_SPLINE_CURVE((1.,1.,1.,1.,1.,1.,1.,1.,1.,1.,1.,1.,1.,1.,1.,1.,
1.,1.,1.,1.,1.,1.,1.,1.,1.,1.,1.,1.,1.,1.,1.,1.,1.,1.,1.,1.,1.,1.,1.,1.,
1.,1.,1.,1.,1.,1.,1.,1.,1.,1.,1.,1.,1.,1.,1.,1.,1.,1.,1.,1.,1.,1.,1.,1.,
1.,1.,1.,1.,1.,1.))
REPRESENTATION_ITEM('')
);
#88=(
BOUNDED_CURVE()
B_SPLINE_CURVE(5,(#23549,#23550,#23551,#23552,#23553,#23554,#23555,#23556,
#23557,#23558,#23559,#23560,#23561,#23562,#23563,#23564,#23565,#23566,#23567,
#23568,#23569,#23570,#23571,#23572,#23573,#23574,#23575,#23576,#23577,#23578,
#23579,#23580,#23581,#23582,#23583,#23584,#23585,#23586,#23587,#23588,#23589,
#23590,#23591,#23592,#23593,#23594,#23595,#23596,#23597,#23598,#23599,#23600,
#23601,#23602,#23603,#23604,#23605,#23606,#23607,#23608,#23609,#23610,#23611,
#23612,#23613,#23614,#23615,#23616,#23617,#23618),.UNSPECIFIED.,.F.,.F.)
B_SPLINE_CURVE_WITH_KNOTS((6,1,1,1,1,1,1,1,1,1,1,1,1,1,1,1,1,1,1,1,1,1,
1,1,1,1,1,1,1,1,1,1,1,1,1,1,1,1,1,1,1,1,1,1,1,1,1,1,1,1,1,1,1,1,1,1,1,1,
1,1,1,1,1,1,1,6),(0.,0.0153846153846154,0.0307692307692308,0.0461538461538462,
0.0615384615384615,0.0769230769230769,0.0923076923076923,0.107692307692308,
0.123076923076923,0.138461538461538,0.153846153846154,0.169230769230769,
0.184615384615385,0.2,0.215384615384615,0.230769230769231,0.246153846153846,
0.261538461538462,0.276923076923077,0.292307692307692,0.307692307692308,
0.323076923076923,0.338461538461538,0.353846153846154,0.369230769230769,
0.384615384615385,0.4,0.415384615384615,0.430769230769231,0.446153846153846,
0.461538461538462,0.476923076923077,0.492307692307692,0.507692307692308,
0.523076923076923,0.538461538461538,0.553846153846154,0.569230769230769,
0.584615384615384,0.6,0.615384615384615,0.63076923076923,0.646153846153846,
0.661538461538461,0.676923076923076,0.692307692307692,0.707692307692307,
0.723076923076922,0.738461538461538,0.753846153846153,0.769230769230768,
0.784615384615384,0.799999999999999,0.815384615384614,0.83076923076923,
0.846153846153845,0.86153846153846,0.876923076923076,0.892307692307691,
0.907692307692306,0.923076923076922,0.938461538461537,0.953846153846152,
0.969230769230768,0.984615384615383,1.),.UNSPECIFIED.)
CURVE()
GEOMETRIC_REPRESENTATION_ITEM()
RATIONAL_B_SPLINE_CURVE((1.,1.,1.,1.,1.,1.,1.,1.,1.,1.,1.,1.,1.,1.,1.,1.,
1.,1.,1.,1.,1.,1.,1.,1.,1.,1.,1.,1.,1.,1.,1.,1.,1.,1.,1.,1.,1.,1.,1.,1.,
1.,1.,1.,1.,1.,1.,1.,1.,1.,1.,1.,1.,1.,1.,1.,1.,1.,1.,1.,1.,1.,1.,1.,1.,
1.,1.,1.,1.,1.,1.))
REPRESENTATION_ITEM('')
);
#89=(
BOUNDED_CURVE()
B_SPLINE_CURVE(5,(#23622,#23623,#23624,#23625,#23626,#23627,#23628,#23629,
#23630,#23631,#23632,#23633,#23634,#23635,#23636,#23637,#23638,#23639,#23640,
#23641,#23642,#23643,#23644,#23645,#23646,#23647,#23648,#23649,#23650,#23651,
#23652,#23653,#23654,#23655,#23656,#23657,#23658,#23659,#23660,#23661,#23662,
#23663,#23664,#23665,#23666,#23667,#23668,#23669,#23670,#23671,#23672,#23673,
#23674,#23675,#23676,#23677,#23678,#23679,#23680,#23681,#23682,#23683,#23684,
#23685,#23686,#23687,#23688,#23689,#23690,#23691),.UNSPECIFIED.,.F.,.F.)
B_SPLINE_CURVE_WITH_KNOTS((6,1,1,1,1,1,1,1,1,1,1,1,1,1,1,1,1,1,1,1,1,1,
1,1,1,1,1,1,1,1,1,1,1,1,1,1,1,1,1,1,1,1,1,1,1,1,1,1,1,1,1,1,1,1,1,1,1,1,
1,1,1,1,1,1,1,6),(0.,0.0153846153846154,0.0307692307692308,0.0461538461538462,
0.0615384615384615,0.0769230769230769,0.0923076923076923,0.107692307692308,
0.123076923076923,0.138461538461538,0.153846153846154,0.169230769230769,
0.184615384615385,0.2,0.215384615384615,0.230769230769231,0.246153846153846,
0.261538461538462,0.276923076923077,0.292307692307692,0.307692307692308,
0.323076923076923,0.338461538461538,0.353846153846154,0.369230769230769,
0.384615384615385,0.4,0.415384615384615,0.430769230769231,0.446153846153846,
0.461538461538462,0.476923076923077,0.492307692307692,0.507692307692308,
0.523076923076923,0.538461538461538,0.553846153846154,0.569230769230769,
0.584615384615384,0.6,0.615384615384615,0.63076923076923,0.646153846153846,
0.661538461538461,0.676923076923076,0.692307692307692,0.707692307692307,
0.723076923076922,0.738461538461538,0.753846153846153,0.769230769230768,
0.784615384615384,0.799999999999999,0.815384615384614,0.83076923076923,
0.846153846153845,0.86153846153846,0.876923076923076,0.892307692307691,
0.907692307692306,0.923076923076922,0.938461538461537,0.953846153846152,
0.969230769230768,0.984615384615383,1.),.UNSPECIFIED.)
CURVE()
GEOMETRIC_REPRESENTATION_ITEM()
RATIONAL_B_SPLINE_CURVE((1.,1.,1.,1.,1.,1.,1.,1.,1.,1.,1.,1.,1.,1.,1.,1.,
1.,1.,1.,1.,1.,1.,1.,1.,1.,1.,1.,1.,1.,1.,1.,1.,1.,1.,1.,1.,1.,1.,1.,1.,
1.,1.,1.,1.,1.,1.,1.,1.,1.,1.,1.,1.,1.,1.,1.,1.,1.,1.,1.,1.,1.,1.,1.,1.,
1.,1.,1.,1.,1.,1.))
REPRESENTATION_ITEM('')
);
#90=(
BOUNDED_CURVE()
B_SPLINE_CURVE(5,(#23694,#23695,#23696,#23697,#23698,#23699,#23700,#23701,
#23702,#23703,#23704,#23705,#23706,#23707,#23708,#23709,#23710,#23711,#23712,
#23713,#23714,#23715,#23716,#23717,#23718,#23719,#23720,#23721,#23722,#23723,
#23724,#23725,#23726,#23727,#23728,#23729,#23730,#23731,#23732,#23733,#23734,
#23735,#23736,#23737,#23738,#23739,#23740,#23741,#23742,#23743,#23744,#23745,
#23746,#23747,#23748,#23749,#23750,#23751,#23752,#23753,#23754,#23755,#23756,
#23757,#23758,#23759,#23760,#23761,#23762,#23763),.UNSPECIFIED.,.F.,.F.)
B_SPLINE_CURVE_WITH_KNOTS((6,1,1,1,1,1,1,1,1,1,1,1,1,1,1,1,1,1,1,1,1,1,
1,1,1,1,1,1,1,1,1,1,1,1,1,1,1,1,1,1,1,1,1,1,1,1,1,1,1,1,1,1,1,1,1,1,1,1,
1,1,1,1,1,1,1,6),(0.,0.0153846153846154,0.0307692307692308,0.0461538461538462,
0.0615384615384615,0.0769230769230769,0.0923076923076923,0.107692307692308,
0.123076923076923,0.138461538461538,0.153846153846154,0.169230769230769,
0.184615384615385,0.2,0.215384615384615,0.230769230769231,0.246153846153846,
0.261538461538462,0.276923076923077,0.292307692307692,0.307692307692308,
0.323076923076923,0.338461538461538,0.353846153846154,0.369230769230769,
0.384615384615385,0.4,0.415384615384615,0.430769230769231,0.446153846153846,
0.461538461538462,0.476923076923077,0.492307692307692,0.507692307692308,
0.523076923076923,0.538461538461538,0.553846153846154,0.569230769230769,
0.584615384615384,0.6,0.615384615384615,0.63076923076923,0.646153846153846,
0.661538461538461,0.676923076923076,0.692307692307692,0.707692307692307,
0.723076923076922,0.738461538461538,0.753846153846153,0.769230769230768,
0.784615384615384,0.799999999999999,0.815384615384614,0.83076923076923,
0.846153846153845,0.86153846153846,0.876923076923076,0.892307692307691,
0.907692307692306,0.923076923076922,0.938461538461537,0.953846153846152,
0.969230769230768,0.984615384615383,1.),.UNSPECIFIED.)
CURVE()
GEOMETRIC_REPRESENTATION_ITEM()
RATIONAL_B_SPLINE_CURVE((1.,1.,1.,1.,1.,1.,1.,1.,1.,1.,1.,1.,1.,1.,1.,1.,
1.,1.,1.,1.,1.,1.,1.,1.,1.,1.,1.,1.,1.,1.,1.,1.,1.,1.,1.,1.,1.,1.,1.,1.,
1.,1.,1.,1.,1.,1.,1.,1.,1.,1.,1.,1.,1.,1.,1.,1.,1.,1.,1.,1.,1.,1.,1.,1.,
1.,1.,1.,1.,1.,1.))
REPRESENTATION_ITEM('')
);
#91=(
BOUNDED_CURVE()
B_SPLINE_CURVE(5,(#23917,#23918,#23919,#23920,#23921,#23922,#23923,#23924,
#23925,#23926,#23927,#23928,#23929,#23930,#23931,#23932,#23933,#23934,#23935,
#23936,#23937,#23938,#23939,#23940,#23941,#23942,#23943,#23944,#23945,#23946,
#23947,#23948,#23949,#23950,#23951,#23952,#23953,#23954,#23955,#23956,#23957,
#23958,#23959,#23960,#23961,#23962,#23963,#23964,#23965,#23966,#23967,#23968,
#23969,#23970,#23971,#23972,#23973,#23974,#23975,#23976,#23977,#23978,#23979,
#23980,#23981,#23982,#23983,#23984,#23985,#23986),.UNSPECIFIED.,.F.,.F.)
B_SPLINE_CURVE_WITH_KNOTS((6,1,1,1,1,1,1,1,1,1,1,1,1,1,1,1,1,1,1,1,1,1,
1,1,1,1,1,1,1,1,1,1,1,1,1,1,1,1,1,1,1,1,1,1,1,1,1,1,1,1,1,1,1,1,1,1,1,1,
1,1,1,1,1,1,1,6),(-1.,-0.984615384615383,-0.969230769230768,-0.953846153846152,
-0.938461538461537,-0.923076923076922,-0.907692307692306,-0.892307692307691,
-0.876923076923076,-0.86153846153846,-0.846153846153845,-0.83076923076923,
-0.815384615384614,-0.799999999999999,-0.784615384615384,-0.769230769230768,
-0.753846153846153,-0.738461538461538,-0.723076923076922,-0.707692307692307,
-0.692307692307692,-0.676923076923076,-0.661538461538461,-0.646153846153846,
-0.63076923076923,-0.615384615384615,-0.6,-0.584615384615384,-0.569230769230769,
-0.553846153846154,-0.538461538461538,-0.523076923076923,-0.507692307692308,
-0.492307692307692,-0.476923076923077,-0.461538461538462,-0.446153846153846,
-0.430769230769231,-0.415384615384615,-0.4,-0.384615384615385,-0.369230769230769,
-0.353846153846154,-0.338461538461538,-0.323076923076923,-0.307692307692308,
-0.292307692307692,-0.276923076923077,-0.261538461538462,-0.246153846153846,
-0.230769230769231,-0.215384615384615,-0.2,-0.184615384615385,-0.169230769230769,
-0.153846153846154,-0.138461538461538,-0.123076923076923,-0.107692307692308,
-0.0923076923076923,-0.0769230769230769,-0.0615384615384615,-0.0461538461538462,
-0.0307692307692308,-0.0153846153846154,0.),.UNSPECIFIED.)
CURVE()
GEOMETRIC_REPRESENTATION_ITEM()
RATIONAL_B_SPLINE_CURVE((1.,1.,1.,1.,1.,1.,1.,1.,1.,1.,1.,1.,1.,1.,1.,1.,
1.,1.,1.,1.,1.,1.,1.,1.,1.,1.,1.,1.,1.,1.,1.,1.,1.,1.,1.,1.,1.,1.,1.,1.,
1.,1.,1.,1.,1.,1.,1.,1.,1.,1.,1.,1.,1.,1.,1.,1.,1.,1.,1.,1.,1.,1.,1.,1.,
1.,1.,1.,1.,1.,1.))
REPRESENTATION_ITEM('')
);
#92=(
BOUNDED_CURVE()
B_SPLINE_CURVE(5,(#24133,#24134,#24135,#24136,#24137,#24138,#24139,#24140,
#24141,#24142,#24143,#24144,#24145,#24146,#24147,#24148,#24149,#24150,#24151,
#24152,#24153,#24154,#24155,#24156,#24157,#24158,#24159,#24160,#24161,#24162,
#24163,#24164,#24165,#24166,#24167,#24168,#24169,#24170,#24171,#24172,#24173,
#24174,#24175,#24176,#24177,#24178,#24179,#24180,#24181,#24182,#24183,#24184,
#24185,#24186,#24187,#24188,#24189,#24190,#24191,#24192,#24193,#24194,#24195,
#24196,#24197,#24198,#24199,#24200,#24201,#24202),.UNSPECIFIED.,.F.,.F.)
B_SPLINE_CURVE_WITH_KNOTS((6,1,1,1,1,1,1,1,1,1,1,1,1,1,1,1,1,1,1,1,1,1,
1,1,1,1,1,1,1,1,1,1,1,1,1,1,1,1,1,1,1,1,1,1,1,1,1,1,1,1,1,1,1,1,1,1,1,1,
1,1,1,1,1,1,1,6),(-1.,-0.984615384615383,-0.969230769230768,-0.953846153846152,
-0.938461538461537,-0.923076923076922,-0.907692307692306,-0.892307692307691,
-0.876923076923076,-0.86153846153846,-0.846153846153845,-0.83076923076923,
-0.815384615384614,-0.799999999999999,-0.784615384615384,-0.769230769230768,
-0.753846153846153,-0.738461538461538,-0.723076923076922,-0.707692307692307,
-0.692307692307692,-0.676923076923076,-0.661538461538461,-0.646153846153846,
-0.63076923076923,-0.615384615384615,-0.6,-0.584615384615384,-0.569230769230769,
-0.553846153846154,-0.538461538461538,-0.523076923076923,-0.507692307692308,
-0.492307692307692,-0.476923076923077,-0.461538461538462,-0.446153846153846,
-0.430769230769231,-0.415384615384615,-0.4,-0.384615384615385,-0.369230769230769,
-0.353846153846154,-0.338461538461538,-0.323076923076923,-0.307692307692308,
-0.292307692307692,-0.276923076923077,-0.261538461538462,-0.246153846153846,
-0.230769230769231,-0.215384615384615,-0.2,-0.184615384615385,-0.169230769230769,
-0.153846153846154,-0.138461538461538,-0.123076923076923,-0.107692307692308,
-0.0923076923076923,-0.0769230769230769,-0.0615384615384615,-0.0461538461538462,
-0.0307692307692308,-0.0153846153846154,0.),.UNSPECIFIED.)
CURVE()
GEOMETRIC_REPRESENTATION_ITEM()
RATIONAL_B_SPLINE_CURVE((1.,1.,1.,1.,1.,1.,1.,1.,1.,1.,1.,1.,1.,1.,1.,1.,
1.,1.,1.,1.,1.,1.,1.,1.,1.,1.,1.,1.,1.,1.,1.,1.,1.,1.,1.,1.,1.,1.,1.,1.,
1.,1.,1.,1.,1.,1.,1.,1.,1.,1.,1.,1.,1.,1.,1.,1.,1.,1.,1.,1.,1.,1.,1.,1.,
1.,1.,1.,1.,1.,1.))
REPRESENTATION_ITEM('')
);
#93=(
BOUNDED_CURVE()
B_SPLINE_CURVE(5,(#24349,#24350,#24351,#24352,#24353,#24354,#24355,#24356,
#24357,#24358,#24359,#24360,#24361,#24362,#24363,#24364,#24365,#24366,#24367,
#24368,#24369,#24370,#24371,#24372,#24373,#24374,#24375,#24376,#24377,#24378,
#24379,#24380,#24381,#24382,#24383,#24384,#24385,#24386,#24387,#24388,#24389,
#24390,#24391,#24392,#24393,#24394,#24395,#24396,#24397,#24398,#24399,#24400,
#24401,#24402,#24403,#24404,#24405,#24406,#24407,#24408,#24409,#24410,#24411,
#24412,#24413,#24414,#24415,#24416,#24417,#24418),.UNSPECIFIED.,.F.,.F.)
B_SPLINE_CURVE_WITH_KNOTS((6,1,1,1,1,1,1,1,1,1,1,1,1,1,1,1,1,1,1,1,1,1,
1,1,1,1,1,1,1,1,1,1,1,1,1,1,1,1,1,1,1,1,1,1,1,1,1,1,1,1,1,1,1,1,1,1,1,1,
1,1,1,1,1,1,1,6),(-1.,-0.984615384615383,-0.969230769230768,-0.953846153846152,
-0.938461538461537,-0.923076923076922,-0.907692307692306,-0.892307692307691,
-0.876923076923076,-0.86153846153846,-0.846153846153845,-0.83076923076923,
-0.815384615384614,-0.799999999999999,-0.784615384615384,-0.769230769230768,
-0.753846153846153,-0.738461538461538,-0.723076923076922,-0.707692307692307,
-0.692307692307692,-0.676923076923076,-0.661538461538461,-0.646153846153846,
-0.63076923076923,-0.615384615384615,-0.6,-0.584615384615384,-0.569230769230769,
-0.553846153846154,-0.538461538461538,-0.523076923076923,-0.507692307692308,
-0.492307692307692,-0.476923076923077,-0.461538461538462,-0.446153846153846,
-0.430769230769231,-0.415384615384615,-0.4,-0.384615384615385,-0.369230769230769,
-0.353846153846154,-0.338461538461538,-0.323076923076923,-0.307692307692308,
-0.292307692307692,-0.276923076923077,-0.261538461538462,-0.246153846153846,
-0.230769230769231,-0.215384615384615,-0.2,-0.184615384615385,-0.169230769230769,
-0.153846153846154,-0.138461538461538,-0.123076923076923,-0.107692307692308,
-0.0923076923076923,-0.0769230769230769,-0.0615384615384615,-0.0461538461538462,
-0.0307692307692308,-0.0153846153846154,0.),.UNSPECIFIED.)
CURVE()
GEOMETRIC_REPRESENTATION_ITEM()
RATIONAL_B_SPLINE_CURVE((1.,1.,1.,1.,1.,1.,1.,1.,1.,1.,1.,1.,1.,1.,1.,1.,
1.,1.,1.,1.,1.,1.,1.,1.,1.,1.,1.,1.,1.,1.,1.,1.,1.,1.,1.,1.,1.,1.,1.,1.,
1.,1.,1.,1.,1.,1.,1.,1.,1.,1.,1.,1.,1.,1.,1.,1.,1.,1.,1.,1.,1.,1.,1.,1.,
1.,1.,1.,1.,1.,1.))
REPRESENTATION_ITEM('')
);
#94=(
BOUNDED_CURVE()
B_SPLINE_CURVE(5,(#24565,#24566,#24567,#24568,#24569,#24570,#24571,#24572,
#24573,#24574,#24575,#24576,#24577,#24578,#24579,#24580,#24581,#24582,#24583,
#24584,#24585,#24586,#24587,#24588,#24589,#24590,#24591,#24592,#24593,#24594,
#24595,#24596,#24597,#24598,#24599,#24600,#24601,#24602,#24603,#24604,#24605,
#24606,#24607,#24608,#24609,#24610,#24611,#24612,#24613,#24614,#24615,#24616,
#24617,#24618,#24619,#24620,#24621,#24622,#24623,#24624,#24625,#24626,#24627,
#24628,#24629,#24630,#24631,#24632,#24633,#24634),.UNSPECIFIED.,.F.,.F.)
B_SPLINE_CURVE_WITH_KNOTS((6,1,1,1,1,1,1,1,1,1,1,1,1,1,1,1,1,1,1,1,1,1,
1,1,1,1,1,1,1,1,1,1,1,1,1,1,1,1,1,1,1,1,1,1,1,1,1,1,1,1,1,1,1,1,1,1,1,1,
1,1,1,1,1,1,1,6),(-1.,-0.984615384615383,-0.969230769230768,-0.953846153846152,
-0.938461538461537,-0.923076923076922,-0.907692307692306,-0.892307692307691,
-0.876923076923076,-0.86153846153846,-0.846153846153845,-0.83076923076923,
-0.815384615384614,-0.799999999999999,-0.784615384615384,-0.769230769230768,
-0.753846153846153,-0.738461538461538,-0.723076923076922,-0.707692307692307,
-0.692307692307692,-0.676923076923076,-0.661538461538461,-0.646153846153846,
-0.63076923076923,-0.615384615384615,-0.6,-0.584615384615384,-0.569230769230769,
-0.553846153846154,-0.538461538461538,-0.523076923076923,-0.507692307692308,
-0.492307692307692,-0.476923076923077,-0.461538461538462,-0.446153846153846,
-0.430769230769231,-0.415384615384615,-0.4,-0.384615384615385,-0.369230769230769,
-0.353846153846154,-0.338461538461538,-0.323076923076923,-0.307692307692308,
-0.292307692307692,-0.276923076923077,-0.261538461538462,-0.246153846153846,
-0.230769230769231,-0.215384615384615,-0.2,-0.184615384615385,-0.169230769230769,
-0.153846153846154,-0.138461538461538,-0.123076923076923,-0.107692307692308,
-0.0923076923076923,-0.0769230769230769,-0.0615384615384615,-0.0461538461538462,
-0.0307692307692308,-0.0153846153846154,0.),.UNSPECIFIED.)
CURVE()
GEOMETRIC_REPRESENTATION_ITEM()
RATIONAL_B_SPLINE_CURVE((1.,1.,1.,1.,1.,1.,1.,1.,1.,1.,1.,1.,1.,1.,1.,1.,
1.,1.,1.,1.,1.,1.,1.,1.,1.,1.,1.,1.,1.,1.,1.,1.,1.,1.,1.,1.,1.,1.,1.,1.,
1.,1.,1.,1.,1.,1.,1.,1.,1.,1.,1.,1.,1.,1.,1.,1.,1.,1.,1.,1.,1.,1.,1.,1.,
1.,1.,1.,1.,1.,1.))
REPRESENTATION_ITEM('')
);
#95=(
BOUNDED_CURVE()
B_SPLINE_CURVE(5,(#24781,#24782,#24783,#24784,#24785,#24786,#24787,#24788,
#24789,#24790,#24791,#24792,#24793,#24794,#24795,#24796,#24797,#24798,#24799,
#24800,#24801,#24802,#24803,#24804,#24805,#24806,#24807,#24808,#24809,#24810,
#24811,#24812,#24813,#24814,#24815,#24816,#24817,#24818,#24819,#24820,#24821,
#24822,#24823,#24824,#24825,#24826,#24827,#24828,#24829,#24830,#24831,#24832,
#24833,#24834,#24835,#24836,#24837,#24838,#24839,#24840,#24841,#24842,#24843,
#24844,#24845,#24846,#24847,#24848,#24849,#24850),.UNSPECIFIED.,.F.,.F.)
B_SPLINE_CURVE_WITH_KNOTS((6,1,1,1,1,1,1,1,1,1,1,1,1,1,1,1,1,1,1,1,1,1,
1,1,1,1,1,1,1,1,1,1,1,1,1,1,1,1,1,1,1,1,1,1,1,1,1,1,1,1,1,1,1,1,1,1,1,1,
1,1,1,1,1,1,1,6),(-1.,-0.984615384615383,-0.969230769230768,-0.953846153846152,
-0.938461538461537,-0.923076923076922,-0.907692307692306,-0.892307692307691,
-0.876923076923076,-0.86153846153846,-0.846153846153845,-0.83076923076923,
-0.815384615384614,-0.799999999999999,-0.784615384615384,-0.769230769230768,
-0.753846153846153,-0.738461538461538,-0.723076923076922,-0.707692307692307,
-0.692307692307692,-0.676923076923076,-0.661538461538461,-0.646153846153846,
-0.63076923076923,-0.615384615384615,-0.6,-0.584615384615384,-0.569230769230769,
-0.553846153846154,-0.538461538461538,-0.523076923076923,-0.507692307692308,
-0.492307692307692,-0.476923076923077,-0.461538461538462,-0.446153846153846,
-0.430769230769231,-0.415384615384615,-0.4,-0.384615384615385,-0.369230769230769,
-0.353846153846154,-0.338461538461538,-0.323076923076923,-0.307692307692308,
-0.292307692307692,-0.276923076923077,-0.261538461538462,-0.246153846153846,
-0.230769230769231,-0.215384615384615,-0.2,-0.184615384615385,-0.169230769230769,
-0.153846153846154,-0.138461538461538,-0.123076923076923,-0.107692307692308,
-0.0923076923076923,-0.0769230769230769,-0.0615384615384615,-0.0461538461538462,
-0.0307692307692308,-0.0153846153846154,0.),.UNSPECIFIED.)
CURVE()
GEOMETRIC_REPRESENTATION_ITEM()
RATIONAL_B_SPLINE_CURVE((1.,1.,1.,1.,1.,1.,1.,1.,1.,1.,1.,1.,1.,1.,1.,1.,
1.,1.,1.,1.,1.,1.,1.,1.,1.,1.,1.,1.,1.,1.,1.,1.,1.,1.,1.,1.,1.,1.,1.,1.,
1.,1.,1.,1.,1.,1.,1.,1.,1.,1.,1.,1.,1.,1.,1.,1.,1.,1.,1.,1.,1.,1.,1.,1.,
1.,1.,1.,1.,1.,1.))
REPRESENTATION_ITEM('')
);
#96=(
BOUNDED_CURVE()
B_SPLINE_CURVE(5,(#24997,#24998,#24999,#25000,#25001,#25002,#25003,#25004,
#25005,#25006,#25007,#25008,#25009,#25010,#25011,#25012,#25013,#25014,#25015,
#25016,#25017,#25018,#25019,#25020,#25021,#25022,#25023,#25024,#25025,#25026,
#25027,#25028,#25029,#25030,#25031,#25032,#25033,#25034,#25035,#25036,#25037,
#25038,#25039,#25040,#25041,#25042,#25043,#25044,#25045,#25046,#25047,#25048,
#25049,#25050,#25051,#25052,#25053,#25054,#25055,#25056,#25057,#25058,#25059,
#25060,#25061,#25062,#25063,#25064,#25065,#25066),.UNSPECIFIED.,.F.,.F.)
B_SPLINE_CURVE_WITH_KNOTS((6,1,1,1,1,1,1,1,1,1,1,1,1,1,1,1,1,1,1,1,1,1,
1,1,1,1,1,1,1,1,1,1,1,1,1,1,1,1,1,1,1,1,1,1,1,1,1,1,1,1,1,1,1,1,1,1,1,1,
1,1,1,1,1,1,1,6),(-1.,-0.984615384615383,-0.969230769230768,-0.953846153846152,
-0.938461538461537,-0.923076923076922,-0.907692307692306,-0.892307692307691,
-0.876923076923076,-0.86153846153846,-0.846153846153845,-0.83076923076923,
-0.815384615384614,-0.799999999999999,-0.784615384615384,-0.769230769230768,
-0.753846153846153,-0.738461538461538,-0.723076923076922,-0.707692307692307,
-0.692307692307692,-0.676923076923076,-0.661538461538461,-0.646153846153846,
-0.63076923076923,-0.615384615384615,-0.6,-0.584615384615384,-0.569230769230769,
-0.553846153846154,-0.538461538461538,-0.523076923076923,-0.507692307692308,
-0.492307692307692,-0.476923076923077,-0.461538461538462,-0.446153846153846,
-0.430769230769231,-0.415384615384615,-0.4,-0.384615384615385,-0.369230769230769,
-0.353846153846154,-0.338461538461538,-0.323076923076923,-0.307692307692308,
-0.292307692307692,-0.276923076923077,-0.261538461538462,-0.246153846153846,
-0.230769230769231,-0.215384615384615,-0.2,-0.184615384615385,-0.169230769230769,
-0.153846153846154,-0.138461538461538,-0.123076923076923,-0.107692307692308,
-0.0923076923076923,-0.0769230769230769,-0.0615384615384615,-0.0461538461538462,
-0.0307692307692308,-0.0153846153846154,0.),.UNSPECIFIED.)
CURVE()
GEOMETRIC_REPRESENTATION_ITEM()
RATIONAL_B_SPLINE_CURVE((1.,1.,1.,1.,1.,1.,1.,1.,1.,1.,1.,1.,1.,1.,1.,1.,
1.,1.,1.,1.,1.,1.,1.,1.,1.,1.,1.,1.,1.,1.,1.,1.,1.,1.,1.,1.,1.,1.,1.,1.,
1.,1.,1.,1.,1.,1.,1.,1.,1.,1.,1.,1.,1.,1.,1.,1.,1.,1.,1.,1.,1.,1.,1.,1.,
1.,1.,1.,1.,1.,1.))
REPRESENTATION_ITEM('')
);
#97=(
BOUNDED_CURVE()
B_SPLINE_CURVE(5,(#25213,#25214,#25215,#25216,#25217,#25218,#25219,#25220,
#25221,#25222,#25223,#25224,#25225,#25226,#25227,#25228,#25229,#25230,#25231,
#25232,#25233,#25234,#25235,#25236,#25237,#25238,#25239,#25240,#25241,#25242,
#25243,#25244,#25245,#25246,#25247,#25248,#25249,#25250,#25251,#25252,#25253,
#25254,#25255,#25256,#25257,#25258,#25259,#25260,#25261,#25262,#25263,#25264,
#25265,#25266,#25267,#25268,#25269,#25270,#25271,#25272,#25273,#25274,#25275,
#25276,#25277,#25278,#25279,#25280,#25281,#25282),.UNSPECIFIED.,.F.,.F.)
B_SPLINE_CURVE_WITH_KNOTS((6,1,1,1,1,1,1,1,1,1,1,1,1,1,1,1,1,1,1,1,1,1,
1,1,1,1,1,1,1,1,1,1,1,1,1,1,1,1,1,1,1,1,1,1,1,1,1,1,1,1,1,1,1,1,1,1,1,1,
1,1,1,1,1,1,1,6),(-1.,-0.984615384615383,-0.969230769230768,-0.953846153846152,
-0.938461538461537,-0.923076923076922,-0.907692307692306,-0.892307692307691,
-0.876923076923076,-0.86153846153846,-0.846153846153845,-0.83076923076923,
-0.815384615384614,-0.799999999999999,-0.784615384615384,-0.769230769230768,
-0.753846153846153,-0.738461538461538,-0.723076923076922,-0.707692307692307,
-0.692307692307692,-0.676923076923076,-0.661538461538461,-0.646153846153846,
-0.63076923076923,-0.615384615384615,-0.6,-0.584615384615384,-0.569230769230769,
-0.553846153846154,-0.538461538461538,-0.523076923076923,-0.507692307692308,
-0.492307692307692,-0.476923076923077,-0.461538461538462,-0.446153846153846,
-0.430769230769231,-0.415384615384615,-0.4,-0.384615384615385,-0.369230769230769,
-0.353846153846154,-0.338461538461538,-0.323076923076923,-0.307692307692308,
-0.292307692307692,-0.276923076923077,-0.261538461538462,-0.246153846153846,
-0.230769230769231,-0.215384615384615,-0.2,-0.184615384615385,-0.169230769230769,
-0.153846153846154,-0.138461538461538,-0.123076923076923,-0.107692307692308,
-0.0923076923076923,-0.0769230769230769,-0.0615384615384615,-0.0461538461538462,
-0.0307692307692308,-0.0153846153846154,0.),.UNSPECIFIED.)
CURVE()
GEOMETRIC_REPRESENTATION_ITEM()
RATIONAL_B_SPLINE_CURVE((1.,1.,1.,1.,1.,1.,1.,1.,1.,1.,1.,1.,1.,1.,1.,1.,
1.,1.,1.,1.,1.,1.,1.,1.,1.,1.,1.,1.,1.,1.,1.,1.,1.,1.,1.,1.,1.,1.,1.,1.,
1.,1.,1.,1.,1.,1.,1.,1.,1.,1.,1.,1.,1.,1.,1.,1.,1.,1.,1.,1.,1.,1.,1.,1.,
1.,1.,1.,1.,1.,1.))
REPRESENTATION_ITEM('')
);
#98=(
BOUNDED_CURVE()
B_SPLINE_CURVE(5,(#25429,#25430,#25431,#25432,#25433,#25434,#25435,#25436,
#25437,#25438,#25439,#25440,#25441,#25442,#25443,#25444,#25445,#25446,#25447,
#25448,#25449,#25450,#25451,#25452,#25453,#25454,#25455,#25456,#25457,#25458,
#25459,#25460,#25461,#25462,#25463,#25464,#25465,#25466,#25467,#25468,#25469,
#25470,#25471,#25472,#25473,#25474,#25475,#25476,#25477,#25478,#25479,#25480,
#25481,#25482,#25483,#25484,#25485,#25486,#25487,#25488,#25489,#25490,#25491,
#25492,#25493,#25494,#25495,#25496,#25497,#25498),.UNSPECIFIED.,.F.,.F.)
B_SPLINE_CURVE_WITH_KNOTS((6,1,1,1,1,1,1,1,1,1,1,1,1,1,1,1,1,1,1,1,1,1,
1,1,1,1,1,1,1,1,1,1,1,1,1,1,1,1,1,1,1,1,1,1,1,1,1,1,1,1,1,1,1,1,1,1,1,1,
1,1,1,1,1,1,1,6),(-1.,-0.984615384615383,-0.969230769230768,-0.953846153846152,
-0.938461538461537,-0.923076923076922,-0.907692307692306,-0.892307692307691,
-0.876923076923076,-0.86153846153846,-0.846153846153845,-0.83076923076923,
-0.815384615384614,-0.799999999999999,-0.784615384615384,-0.769230769230768,
-0.753846153846153,-0.738461538461538,-0.723076923076922,-0.707692307692307,
-0.692307692307692,-0.676923076923076,-0.661538461538461,-0.646153846153846,
-0.63076923076923,-0.615384615384615,-0.6,-0.584615384615384,-0.569230769230769,
-0.553846153846154,-0.538461538461538,-0.523076923076923,-0.507692307692308,
-0.492307692307692,-0.476923076923077,-0.461538461538462,-0.446153846153846,
-0.430769230769231,-0.415384615384615,-0.4,-0.384615384615385,-0.369230769230769,
-0.353846153846154,-0.338461538461538,-0.323076923076923,-0.307692307692308,
-0.292307692307692,-0.276923076923077,-0.261538461538462,-0.246153846153846,
-0.230769230769231,-0.215384615384615,-0.2,-0.184615384615385,-0.169230769230769,
-0.153846153846154,-0.138461538461538,-0.123076923076923,-0.107692307692308,
-0.0923076923076923,-0.0769230769230769,-0.0615384615384615,-0.0461538461538462,
-0.0307692307692308,-0.0153846153846154,0.),.UNSPECIFIED.)
CURVE()
GEOMETRIC_REPRESENTATION_ITEM()
RATIONAL_B_SPLINE_CURVE((1.,1.,1.,1.,1.,1.,1.,1.,1.,1.,1.,1.,1.,1.,1.,1.,
1.,1.,1.,1.,1.,1.,1.,1.,1.,1.,1.,1.,1.,1.,1.,1.,1.,1.,1.,1.,1.,1.,1.,1.,
1.,1.,1.,1.,1.,1.,1.,1.,1.,1.,1.,1.,1.,1.,1.,1.,1.,1.,1.,1.,1.,1.,1.,1.,
1.,1.,1.,1.,1.,1.))
REPRESENTATION_ITEM('')
);
#99=(
BOUNDED_CURVE()
B_SPLINE_CURVE(5,(#25645,#25646,#25647,#25648,#25649,#25650,#25651,#25652,
#25653,#25654,#25655,#25656,#25657,#25658,#25659,#25660,#25661,#25662,#25663,
#25664,#25665,#25666,#25667,#25668,#25669,#25670,#25671,#25672,#25673,#25674,
#25675,#25676,#25677,#25678,#25679,#25680,#25681,#25682,#25683,#25684,#25685,
#25686,#25687,#25688,#25689,#25690,#25691,#25692,#25693,#25694,#25695,#25696,
#25697,#25698,#25699,#25700,#25701,#25702,#25703,#25704,#25705,#25706,#25707,
#25708,#25709,#25710,#25711,#25712,#25713,#25714),.UNSPECIFIED.,.F.,.F.)
B_SPLINE_CURVE_WITH_KNOTS((6,1,1,1,1,1,1,1,1,1,1,1,1,1,1,1,1,1,1,1,1,1,
1,1,1,1,1,1,1,1,1,1,1,1,1,1,1,1,1,1,1,1,1,1,1,1,1,1,1,1,1,1,1,1,1,1,1,1,
1,1,1,1,1,1,1,6),(-1.,-0.984615384615383,-0.969230769230768,-0.953846153846152,
-0.938461538461537,-0.923076923076922,-0.907692307692306,-0.892307692307691,
-0.876923076923076,-0.86153846153846,-0.846153846153845,-0.83076923076923,
-0.815384615384614,-0.799999999999999,-0.784615384615384,-0.769230769230768,
-0.753846153846153,-0.738461538461538,-0.723076923076922,-0.707692307692307,
-0.692307692307692,-0.676923076923076,-0.661538461538461,-0.646153846153846,
-0.63076923076923,-0.615384615384615,-0.6,-0.584615384615384,-0.569230769230769,
-0.553846153846154,-0.538461538461538,-0.523076923076923,-0.507692307692308,
-0.492307692307692,-0.476923076923077,-0.461538461538462,-0.446153846153846,
-0.430769230769231,-0.415384615384615,-0.4,-0.384615384615385,-0.369230769230769,
-0.353846153846154,-0.338461538461538,-0.323076923076923,-0.307692307692308,
-0.292307692307692,-0.276923076923077,-0.261538461538462,-0.246153846153846,
-0.230769230769231,-0.215384615384615,-0.2,-0.184615384615385,-0.169230769230769,
-0.153846153846154,-0.138461538461538,-0.123076923076923,-0.107692307692308,
-0.0923076923076923,-0.0769230769230769,-0.0615384615384615,-0.0461538461538462,
-0.0307692307692308,-0.0153846153846154,0.),.UNSPECIFIED.)
CURVE()
GEOMETRIC_REPRESENTATION_ITEM()
RATIONAL_B_SPLINE_CURVE((1.,1.,1.,1.,1.,1.,1.,1.,1.,1.,1.,1.,1.,1.,1.,1.,
1.,1.,1.,1.,1.,1.,1.,1.,1.,1.,1.,1.,1.,1.,1.,1.,1.,1.,1.,1.,1.,1.,1.,1.,
1.,1.,1.,1.,1.,1.,1.,1.,1.,1.,1.,1.,1.,1.,1.,1.,1.,1.,1.,1.,1.,1.,1.,1.,
1.,1.,1.,1.,1.,1.))
REPRESENTATION_ITEM('')
);
#100=(
BOUNDED_CURVE()
B_SPLINE_CURVE(5,(#25861,#25862,#25863,#25864,#25865,#25866,#25867,#25868,
#25869,#25870,#25871,#25872,#25873,#25874,#25875,#25876,#25877,#25878,#25879,
#25880,#25881,#25882,#25883,#25884,#25885,#25886,#25887,#25888,#25889,#25890,
#25891,#25892,#25893,#25894,#25895,#25896,#25897,#25898,#25899,#25900,#25901,
#25902,#25903,#25904,#25905,#25906,#25907,#25908,#25909,#25910,#25911,#25912,
#25913,#25914,#25915,#25916,#25917,#25918,#25919,#25920,#25921,#25922,#25923,
#25924,#25925,#25926,#25927,#25928,#25929,#25930),.UNSPECIFIED.,.F.,.F.)
B_SPLINE_CURVE_WITH_KNOTS((6,1,1,1,1,1,1,1,1,1,1,1,1,1,1,1,1,1,1,1,1,1,
1,1,1,1,1,1,1,1,1,1,1,1,1,1,1,1,1,1,1,1,1,1,1,1,1,1,1,1,1,1,1,1,1,1,1,1,
1,1,1,1,1,1,1,6),(-1.,-0.984615384615383,-0.969230769230768,-0.953846153846152,
-0.938461538461537,-0.923076923076922,-0.907692307692306,-0.892307692307691,
-0.876923076923076,-0.86153846153846,-0.846153846153845,-0.83076923076923,
-0.815384615384614,-0.799999999999999,-0.784615384615384,-0.769230769230768,
-0.753846153846153,-0.738461538461538,-0.723076923076922,-0.707692307692307,
-0.692307692307692,-0.676923076923076,-0.661538461538461,-0.646153846153846,
-0.63076923076923,-0.615384615384615,-0.6,-0.584615384615384,-0.569230769230769,
-0.553846153846154,-0.538461538461538,-0.523076923076923,-0.507692307692308,
-0.492307692307692,-0.476923076923077,-0.461538461538462,-0.446153846153846,
-0.430769230769231,-0.415384615384615,-0.4,-0.384615384615385,-0.369230769230769,
-0.353846153846154,-0.338461538461538,-0.323076923076923,-0.307692307692308,
-0.292307692307692,-0.276923076923077,-0.261538461538462,-0.246153846153846,
-0.230769230769231,-0.215384615384615,-0.2,-0.184615384615385,-0.169230769230769,
-0.153846153846154,-0.138461538461538,-0.123076923076923,-0.107692307692308,
-0.0923076923076923,-0.0769230769230769,-0.0615384615384615,-0.0461538461538462,
-0.0307692307692308,-0.0153846153846154,0.),.UNSPECIFIED.)
CURVE()
GEOMETRIC_REPRESENTATION_ITEM()
RATIONAL_B_SPLINE_CURVE((1.,1.,1.,1.,1.,1.,1.,1.,1.,1.,1.,1.,1.,1.,1.,1.,
1.,1.,1.,1.,1.,1.,1.,1.,1.,1.,1.,1.,1.,1.,1.,1.,1.,1.,1.,1.,1.,1.,1.,1.,
1.,1.,1.,1.,1.,1.,1.,1.,1.,1.,1.,1.,1.,1.,1.,1.,1.,1.,1.,1.,1.,1.,1.,1.,
1.,1.,1.,1.,1.,1.))
REPRESENTATION_ITEM('')
);
#101=(
BOUNDED_CURVE()
B_SPLINE_CURVE(5,(#26077,#26078,#26079,#26080,#26081,#26082,#26083,#26084,
#26085,#26086,#26087,#26088,#26089,#26090,#26091,#26092,#26093,#26094,#26095,
#26096,#26097,#26098,#26099,#26100,#26101,#26102,#26103,#26104,#26105,#26106,
#26107,#26108,#26109,#26110,#26111,#26112,#26113,#26114,#26115,#26116,#26117,
#26118,#26119,#26120,#26121,#26122,#26123,#26124,#26125,#26126,#26127,#26128,
#26129,#26130,#26131,#26132,#26133,#26134,#26135,#26136,#26137,#26138,#26139,
#26140,#26141,#26142,#26143,#26144,#26145,#26146),.UNSPECIFIED.,.F.,.F.)
B_SPLINE_CURVE_WITH_KNOTS((6,1,1,1,1,1,1,1,1,1,1,1,1,1,1,1,1,1,1,1,1,1,
1,1,1,1,1,1,1,1,1,1,1,1,1,1,1,1,1,1,1,1,1,1,1,1,1,1,1,1,1,1,1,1,1,1,1,1,
1,1,1,1,1,1,1,6),(-1.,-0.984615384615383,-0.969230769230768,-0.953846153846152,
-0.938461538461537,-0.923076923076922,-0.907692307692306,-0.892307692307691,
-0.876923076923076,-0.86153846153846,-0.846153846153845,-0.83076923076923,
-0.815384615384614,-0.799999999999999,-0.784615384615384,-0.769230769230768,
-0.753846153846153,-0.738461538461538,-0.723076923076922,-0.707692307692307,
-0.692307692307692,-0.676923076923076,-0.661538461538461,-0.646153846153846,
-0.63076923076923,-0.615384615384615,-0.6,-0.584615384615384,-0.569230769230769,
-0.553846153846154,-0.538461538461538,-0.523076923076923,-0.507692307692308,
-0.492307692307692,-0.476923076923077,-0.461538461538462,-0.446153846153846,
-0.430769230769231,-0.415384615384615,-0.4,-0.384615384615385,-0.369230769230769,
-0.353846153846154,-0.338461538461538,-0.323076923076923,-0.307692307692308,
-0.292307692307692,-0.276923076923077,-0.261538461538462,-0.246153846153846,
-0.230769230769231,-0.215384615384615,-0.2,-0.184615384615385,-0.169230769230769,
-0.153846153846154,-0.138461538461538,-0.123076923076923,-0.107692307692308,
-0.0923076923076923,-0.0769230769230769,-0.0615384615384615,-0.0461538461538462,
-0.0307692307692308,-0.0153846153846154,0.),.UNSPECIFIED.)
CURVE()
GEOMETRIC_REPRESENTATION_ITEM()
RATIONAL_B_SPLINE_CURVE((1.,1.,1.,1.,1.,1.,1.,1.,1.,1.,1.,1.,1.,1.,1.,1.,
1.,1.,1.,1.,1.,1.,1.,1.,1.,1.,1.,1.,1.,1.,1.,1.,1.,1.,1.,1.,1.,1.,1.,1.,
1.,1.,1.,1.,1.,1.,1.,1.,1.,1.,1.,1.,1.,1.,1.,1.,1.,1.,1.,1.,1.,1.,1.,1.,
1.,1.,1.,1.,1.,1.))
REPRESENTATION_ITEM('')
);
#102=(
BOUNDED_CURVE()
B_SPLINE_CURVE(5,(#26293,#26294,#26295,#26296,#26297,#26298,#26299,#26300,
#26301,#26302,#26303,#26304,#26305,#26306,#26307,#26308,#26309,#26310,#26311,
#26312,#26313,#26314,#26315,#26316,#26317,#26318,#26319,#26320,#26321,#26322,
#26323,#26324,#26325,#26326,#26327,#26328,#26329,#26330,#26331,#26332,#26333,
#26334,#26335,#26336,#26337,#26338,#26339,#26340,#26341,#26342,#26343,#26344,
#26345,#26346,#26347,#26348,#26349,#26350,#26351,#26352,#26353,#26354,#26355,
#26356,#26357,#26358,#26359,#26360,#26361,#26362),.UNSPECIFIED.,.F.,.F.)
B_SPLINE_CURVE_WITH_KNOTS((6,1,1,1,1,1,1,1,1,1,1,1,1,1,1,1,1,1,1,1,1,1,
1,1,1,1,1,1,1,1,1,1,1,1,1,1,1,1,1,1,1,1,1,1,1,1,1,1,1,1,1,1,1,1,1,1,1,1,
1,1,1,1,1,1,1,6),(-1.,-0.984615384615383,-0.969230769230768,-0.953846153846152,
-0.938461538461537,-0.923076923076922,-0.907692307692306,-0.892307692307691,
-0.876923076923076,-0.86153846153846,-0.846153846153845,-0.83076923076923,
-0.815384615384614,-0.799999999999999,-0.784615384615384,-0.769230769230768,
-0.753846153846153,-0.738461538461538,-0.723076923076922,-0.707692307692307,
-0.692307692307692,-0.676923076923076,-0.661538461538461,-0.646153846153846,
-0.63076923076923,-0.615384615384615,-0.6,-0.584615384615384,-0.569230769230769,
-0.553846153846154,-0.538461538461538,-0.523076923076923,-0.507692307692308,
-0.492307692307692,-0.476923076923077,-0.461538461538462,-0.446153846153846,
-0.430769230769231,-0.415384615384615,-0.4,-0.384615384615385,-0.369230769230769,
-0.353846153846154,-0.338461538461538,-0.323076923076923,-0.307692307692308,
-0.292307692307692,-0.276923076923077,-0.261538461538462,-0.246153846153846,
-0.230769230769231,-0.215384615384615,-0.2,-0.184615384615385,-0.169230769230769,
-0.153846153846154,-0.138461538461538,-0.123076923076923,-0.107692307692308,
-0.0923076923076923,-0.0769230769230769,-0.0615384615384615,-0.0461538461538462,
-0.0307692307692308,-0.0153846153846154,0.),.UNSPECIFIED.)
CURVE()
GEOMETRIC_REPRESENTATION_ITEM()
RATIONAL_B_SPLINE_CURVE((1.,1.,1.,1.,1.,1.,1.,1.,1.,1.,1.,1.,1.,1.,1.,1.,
1.,1.,1.,1.,1.,1.,1.,1.,1.,1.,1.,1.,1.,1.,1.,1.,1.,1.,1.,1.,1.,1.,1.,1.,
1.,1.,1.,1.,1.,1.,1.,1.,1.,1.,1.,1.,1.,1.,1.,1.,1.,1.,1.,1.,1.,1.,1.,1.,
1.,1.,1.,1.,1.,1.))
REPRESENTATION_ITEM('')
);
#103=(
BOUNDED_CURVE()
B_SPLINE_CURVE(5,(#26509,#26510,#26511,#26512,#26513,#26514,#26515,#26516,
#26517,#26518,#26519,#26520,#26521,#26522,#26523,#26524,#26525,#26526,#26527,
#26528,#26529,#26530,#26531,#26532,#26533,#26534,#26535,#26536,#26537,#26538,
#26539,#26540,#26541,#26542,#26543,#26544,#26545,#26546,#26547,#26548,#26549,
#26550,#26551,#26552,#26553,#26554,#26555,#26556,#26557,#26558,#26559,#26560,
#26561,#26562,#26563,#26564,#26565,#26566,#26567,#26568,#26569,#26570,#26571,
#26572,#26573,#26574,#26575,#26576,#26577,#26578),.UNSPECIFIED.,.F.,.F.)
B_SPLINE_CURVE_WITH_KNOTS((6,1,1,1,1,1,1,1,1,1,1,1,1,1,1,1,1,1,1,1,1,1,
1,1,1,1,1,1,1,1,1,1,1,1,1,1,1,1,1,1,1,1,1,1,1,1,1,1,1,1,1,1,1,1,1,1,1,1,
1,1,1,1,1,1,1,6),(-1.,-0.984615384615383,-0.969230769230768,-0.953846153846152,
-0.938461538461537,-0.923076923076922,-0.907692307692306,-0.892307692307691,
-0.876923076923076,-0.86153846153846,-0.846153846153845,-0.83076923076923,
-0.815384615384614,-0.799999999999999,-0.784615384615384,-0.769230769230768,
-0.753846153846153,-0.738461538461538,-0.723076923076922,-0.707692307692307,
-0.692307692307692,-0.676923076923076,-0.661538461538461,-0.646153846153846,
-0.63076923076923,-0.615384615384615,-0.6,-0.584615384615384,-0.569230769230769,
-0.553846153846154,-0.538461538461538,-0.523076923076923,-0.507692307692308,
-0.492307692307692,-0.476923076923077,-0.461538461538462,-0.446153846153846,
-0.430769230769231,-0.415384615384615,-0.4,-0.384615384615385,-0.369230769230769,
-0.353846153846154,-0.338461538461538,-0.323076923076923,-0.307692307692308,
-0.292307692307692,-0.276923076923077,-0.261538461538462,-0.246153846153846,
-0.230769230769231,-0.215384615384615,-0.2,-0.184615384615385,-0.169230769230769,
-0.153846153846154,-0.138461538461538,-0.123076923076923,-0.107692307692308,
-0.0923076923076923,-0.0769230769230769,-0.0615384615384615,-0.0461538461538462,
-0.0307692307692308,-0.0153846153846154,0.),.UNSPECIFIED.)
CURVE()
GEOMETRIC_REPRESENTATION_ITEM()
RATIONAL_B_SPLINE_CURVE((1.,1.,1.,1.,1.,1.,1.,1.,1.,1.,1.,1.,1.,1.,1.,1.,
1.,1.,1.,1.,1.,1.,1.,1.,1.,1.,1.,1.,1.,1.,1.,1.,1.,1.,1.,1.,1.,1.,1.,1.,
1.,1.,1.,1.,1.,1.,1.,1.,1.,1.,1.,1.,1.,1.,1.,1.,1.,1.,1.,1.,1.,1.,1.,1.,
1.,1.,1.,1.,1.,1.))
REPRESENTATION_ITEM('')
);
#104=(
BOUNDED_CURVE()
B_SPLINE_CURVE(5,(#26725,#26726,#26727,#26728,#26729,#26730,#26731,#26732,
#26733,#26734,#26735,#26736,#26737,#26738,#26739,#26740,#26741,#26742,#26743,
#26744,#26745,#26746,#26747,#26748,#26749,#26750,#26751,#26752,#26753,#26754,
#26755,#26756,#26757,#26758,#26759,#26760,#26761,#26762,#26763,#26764,#26765,
#26766,#26767,#26768,#26769,#26770,#26771,#26772,#26773,#26774,#26775,#26776,
#26777,#26778,#26779,#26780,#26781,#26782,#26783,#26784,#26785,#26786,#26787,
#26788,#26789,#26790,#26791,#26792,#26793,#26794),.UNSPECIFIED.,.F.,.F.)
B_SPLINE_CURVE_WITH_KNOTS((6,1,1,1,1,1,1,1,1,1,1,1,1,1,1,1,1,1,1,1,1,1,
1,1,1,1,1,1,1,1,1,1,1,1,1,1,1,1,1,1,1,1,1,1,1,1,1,1,1,1,1,1,1,1,1,1,1,1,
1,1,1,1,1,1,1,6),(-1.,-0.984615384615383,-0.969230769230768,-0.953846153846152,
-0.938461538461537,-0.923076923076922,-0.907692307692306,-0.892307692307691,
-0.876923076923076,-0.86153846153846,-0.846153846153845,-0.83076923076923,
-0.815384615384614,-0.799999999999999,-0.784615384615384,-0.769230769230768,
-0.753846153846153,-0.738461538461538,-0.723076923076922,-0.707692307692307,
-0.692307692307692,-0.676923076923076,-0.661538461538461,-0.646153846153846,
-0.63076923076923,-0.615384615384615,-0.6,-0.584615384615384,-0.569230769230769,
-0.553846153846154,-0.538461538461538,-0.523076923076923,-0.507692307692308,
-0.492307692307692,-0.476923076923077,-0.461538461538462,-0.446153846153846,
-0.430769230769231,-0.415384615384615,-0.4,-0.384615384615385,-0.369230769230769,
-0.353846153846154,-0.338461538461538,-0.323076923076923,-0.307692307692308,
-0.292307692307692,-0.276923076923077,-0.261538461538462,-0.246153846153846,
-0.230769230769231,-0.215384615384615,-0.2,-0.184615384615385,-0.169230769230769,
-0.153846153846154,-0.138461538461538,-0.123076923076923,-0.107692307692308,
-0.0923076923076923,-0.0769230769230769,-0.0615384615384615,-0.0461538461538462,
-0.0307692307692308,-0.0153846153846154,0.),.UNSPECIFIED.)
CURVE()
GEOMETRIC_REPRESENTATION_ITEM()
RATIONAL_B_SPLINE_CURVE((1.,1.,1.,1.,1.,1.,1.,1.,1.,1.,1.,1.,1.,1.,1.,1.,
1.,1.,1.,1.,1.,1.,1.,1.,1.,1.,1.,1.,1.,1.,1.,1.,1.,1.,1.,1.,1.,1.,1.,1.,
1.,1.,1.,1.,1.,1.,1.,1.,1.,1.,1.,1.,1.,1.,1.,1.,1.,1.,1.,1.,1.,1.,1.,1.,
1.,1.,1.,1.,1.,1.))
REPRESENTATION_ITEM('')
);
#105=(
BOUNDED_CURVE()
B_SPLINE_CURVE(5,(#26941,#26942,#26943,#26944,#26945,#26946,#26947,#26948,
#26949,#26950,#26951,#26952,#26953,#26954,#26955,#26956,#26957,#26958,#26959,
#26960,#26961,#26962,#26963,#26964,#26965,#26966,#26967,#26968,#26969,#26970,
#26971,#26972,#26973,#26974,#26975,#26976,#26977,#26978,#26979,#26980,#26981,
#26982,#26983,#26984,#26985,#26986,#26987,#26988,#26989,#26990,#26991,#26992,
#26993,#26994,#26995,#26996,#26997,#26998,#26999,#27000,#27001,#27002,#27003,
#27004,#27005,#27006,#27007,#27008,#27009,#27010),.UNSPECIFIED.,.F.,.F.)
B_SPLINE_CURVE_WITH_KNOTS((6,1,1,1,1,1,1,1,1,1,1,1,1,1,1,1,1,1,1,1,1,1,
1,1,1,1,1,1,1,1,1,1,1,1,1,1,1,1,1,1,1,1,1,1,1,1,1,1,1,1,1,1,1,1,1,1,1,1,
1,1,1,1,1,1,1,6),(-1.,-0.984615384615383,-0.969230769230768,-0.953846153846152,
-0.938461538461537,-0.923076923076922,-0.907692307692306,-0.892307692307691,
-0.876923076923076,-0.86153846153846,-0.846153846153845,-0.83076923076923,
-0.815384615384614,-0.799999999999999,-0.784615384615384,-0.769230769230768,
-0.753846153846153,-0.738461538461538,-0.723076923076922,-0.707692307692307,
-0.692307692307692,-0.676923076923076,-0.661538461538461,-0.646153846153846,
-0.63076923076923,-0.615384615384615,-0.6,-0.584615384615384,-0.569230769230769,
-0.553846153846154,-0.538461538461538,-0.523076923076923,-0.507692307692308,
-0.492307692307692,-0.476923076923077,-0.461538461538462,-0.446153846153846,
-0.430769230769231,-0.415384615384615,-0.4,-0.384615384615385,-0.369230769230769,
-0.353846153846154,-0.338461538461538,-0.323076923076923,-0.307692307692308,
-0.292307692307692,-0.276923076923077,-0.261538461538462,-0.246153846153846,
-0.230769230769231,-0.215384615384615,-0.2,-0.184615384615385,-0.169230769230769,
-0.153846153846154,-0.138461538461538,-0.123076923076923,-0.107692307692308,
-0.0923076923076923,-0.0769230769230769,-0.0615384615384615,-0.0461538461538462,
-0.0307692307692308,-0.0153846153846154,0.),.UNSPECIFIED.)
CURVE()
GEOMETRIC_REPRESENTATION_ITEM()
RATIONAL_B_SPLINE_CURVE((1.,1.,1.,1.,1.,1.,1.,1.,1.,1.,1.,1.,1.,1.,1.,1.,
1.,1.,1.,1.,1.,1.,1.,1.,1.,1.,1.,1.,1.,1.,1.,1.,1.,1.,1.,1.,1.,1.,1.,1.,
1.,1.,1.,1.,1.,1.,1.,1.,1.,1.,1.,1.,1.,1.,1.,1.,1.,1.,1.,1.,1.,1.,1.,1.,
1.,1.,1.,1.,1.,1.))
REPRESENTATION_ITEM('')
);
#106=(
BOUNDED_CURVE()
B_SPLINE_CURVE(5,(#27157,#27158,#27159,#27160,#27161,#27162,#27163,#27164,
#27165,#27166,#27167,#27168,#27169,#27170,#27171,#27172,#27173,#27174,#27175,
#27176,#27177,#27178,#27179,#27180,#27181,#27182,#27183,#27184,#27185,#27186,
#27187,#27188,#27189,#27190,#27191,#27192,#27193,#27194,#27195,#27196,#27197,
#27198,#27199,#27200,#27201,#27202,#27203,#27204,#27205,#27206,#27207,#27208,
#27209,#27210,#27211,#27212,#27213,#27214,#27215,#27216,#27217,#27218,#27219,
#27220,#27221,#27222,#27223,#27224,#27225,#27226),.UNSPECIFIED.,.F.,.F.)
B_SPLINE_CURVE_WITH_KNOTS((6,1,1,1,1,1,1,1,1,1,1,1,1,1,1,1,1,1,1,1,1,1,
1,1,1,1,1,1,1,1,1,1,1,1,1,1,1,1,1,1,1,1,1,1,1,1,1,1,1,1,1,1,1,1,1,1,1,1,
1,1,1,1,1,1,1,6),(-1.,-0.984615384615383,-0.969230769230768,-0.953846153846152,
-0.938461538461537,-0.923076923076922,-0.907692307692306,-0.892307692307691,
-0.876923076923076,-0.86153846153846,-0.846153846153845,-0.83076923076923,
-0.815384615384614,-0.799999999999999,-0.784615384615384,-0.769230769230768,
-0.753846153846153,-0.738461538461538,-0.723076923076922,-0.707692307692307,
-0.692307692307692,-0.676923076923076,-0.661538461538461,-0.646153846153846,
-0.63076923076923,-0.615384615384615,-0.6,-0.584615384615384,-0.569230769230769,
-0.553846153846154,-0.538461538461538,-0.523076923076923,-0.507692307692308,
-0.492307692307692,-0.476923076923077,-0.461538461538462,-0.446153846153846,
-0.430769230769231,-0.415384615384615,-0.4,-0.384615384615385,-0.369230769230769,
-0.353846153846154,-0.338461538461538,-0.323076923076923,-0.307692307692308,
-0.292307692307692,-0.276923076923077,-0.261538461538462,-0.246153846153846,
-0.230769230769231,-0.215384615384615,-0.2,-0.184615384615385,-0.169230769230769,
-0.153846153846154,-0.138461538461538,-0.123076923076923,-0.107692307692308,
-0.0923076923076923,-0.0769230769230769,-0.0615384615384615,-0.0461538461538462,
-0.0307692307692308,-0.0153846153846154,0.),.UNSPECIFIED.)
CURVE()
GEOMETRIC_REPRESENTATION_ITEM()
RATIONAL_B_SPLINE_CURVE((1.,1.,1.,1.,1.,1.,1.,1.,1.,1.,1.,1.,1.,1.,1.,1.,
1.,1.,1.,1.,1.,1.,1.,1.,1.,1.,1.,1.,1.,1.,1.,1.,1.,1.,1.,1.,1.,1.,1.,1.,
1.,1.,1.,1.,1.,1.,1.,1.,1.,1.,1.,1.,1.,1.,1.,1.,1.,1.,1.,1.,1.,1.,1.,1.,
1.,1.,1.,1.,1.,1.))
REPRESENTATION_ITEM('')
);
#107=(
BOUNDED_CURVE()
B_SPLINE_CURVE(5,(#27373,#27374,#27375,#27376,#27377,#27378,#27379,#27380,
#27381,#27382,#27383,#27384,#27385,#27386,#27387,#27388,#27389,#27390,#27391,
#27392,#27393,#27394,#27395,#27396,#27397,#27398,#27399,#27400,#27401,#27402,
#27403,#27404,#27405,#27406,#27407,#27408,#27409,#27410,#27411,#27412,#27413,
#27414,#27415,#27416,#27417,#27418,#27419,#27420,#27421,#27422,#27423,#27424,
#27425,#27426,#27427,#27428,#27429,#27430,#27431,#27432,#27433,#27434,#27435,
#27436,#27437,#27438,#27439,#27440,#27441,#27442),.UNSPECIFIED.,.F.,.F.)
B_SPLINE_CURVE_WITH_KNOTS((6,1,1,1,1,1,1,1,1,1,1,1,1,1,1,1,1,1,1,1,1,1,
1,1,1,1,1,1,1,1,1,1,1,1,1,1,1,1,1,1,1,1,1,1,1,1,1,1,1,1,1,1,1,1,1,1,1,1,
1,1,1,1,1,1,1,6),(-1.,-0.984615384615383,-0.969230769230768,-0.953846153846152,
-0.938461538461537,-0.923076923076922,-0.907692307692306,-0.892307692307691,
-0.876923076923076,-0.86153846153846,-0.846153846153845,-0.83076923076923,
-0.815384615384614,-0.799999999999999,-0.784615384615384,-0.769230769230768,
-0.753846153846153,-0.738461538461538,-0.723076923076922,-0.707692307692307,
-0.692307692307692,-0.676923076923076,-0.661538461538461,-0.646153846153846,
-0.63076923076923,-0.615384615384615,-0.6,-0.584615384615384,-0.569230769230769,
-0.553846153846154,-0.538461538461538,-0.523076923076923,-0.507692307692308,
-0.492307692307692,-0.476923076923077,-0.461538461538462,-0.446153846153846,
-0.430769230769231,-0.415384615384615,-0.4,-0.384615384615385,-0.369230769230769,
-0.353846153846154,-0.338461538461538,-0.323076923076923,-0.307692307692308,
-0.292307692307692,-0.276923076923077,-0.261538461538462,-0.246153846153846,
-0.230769230769231,-0.215384615384615,-0.2,-0.184615384615385,-0.169230769230769,
-0.153846153846154,-0.138461538461538,-0.123076923076923,-0.107692307692308,
-0.0923076923076923,-0.0769230769230769,-0.0615384615384615,-0.0461538461538462,
-0.0307692307692308,-0.0153846153846154,0.),.UNSPECIFIED.)
CURVE()
GEOMETRIC_REPRESENTATION_ITEM()
RATIONAL_B_SPLINE_CURVE((1.,1.,1.,1.,1.,1.,1.,1.,1.,1.,1.,1.,1.,1.,1.,1.,
1.,1.,1.,1.,1.,1.,1.,1.,1.,1.,1.,1.,1.,1.,1.,1.,1.,1.,1.,1.,1.,1.,1.,1.,
1.,1.,1.,1.,1.,1.,1.,1.,1.,1.,1.,1.,1.,1.,1.,1.,1.,1.,1.,1.,1.,1.,1.,1.,
1.,1.,1.,1.,1.,1.))
REPRESENTATION_ITEM('')
);
#108=(
BOUNDED_CURVE()
B_SPLINE_CURVE(5,(#27589,#27590,#27591,#27592,#27593,#27594,#27595,#27596,
#27597,#27598,#27599,#27600,#27601,#27602,#27603,#27604,#27605,#27606,#27607,
#27608,#27609,#27610,#27611,#27612,#27613,#27614,#27615,#27616,#27617,#27618,
#27619,#27620,#27621,#27622,#27623,#27624,#27625,#27626,#27627,#27628,#27629,
#27630,#27631,#27632,#27633,#27634,#27635,#27636,#27637,#27638,#27639,#27640,
#27641,#27642,#27643,#27644,#27645,#27646,#27647,#27648,#27649,#27650,#27651,
#27652,#27653,#27654,#27655,#27656,#27657,#27658),.UNSPECIFIED.,.F.,.F.)
B_SPLINE_CURVE_WITH_KNOTS((6,1,1,1,1,1,1,1,1,1,1,1,1,1,1,1,1,1,1,1,1,1,
1,1,1,1,1,1,1,1,1,1,1,1,1,1,1,1,1,1,1,1,1,1,1,1,1,1,1,1,1,1,1,1,1,1,1,1,
1,1,1,1,1,1,1,6),(-1.,-0.984615384615383,-0.969230769230768,-0.953846153846152,
-0.938461538461537,-0.923076923076922,-0.907692307692306,-0.892307692307691,
-0.876923076923076,-0.86153846153846,-0.846153846153845,-0.83076923076923,
-0.815384615384614,-0.799999999999999,-0.784615384615384,-0.769230769230768,
-0.753846153846153,-0.738461538461538,-0.723076923076922,-0.707692307692307,
-0.692307692307692,-0.676923076923076,-0.661538461538461,-0.646153846153846,
-0.63076923076923,-0.615384615384615,-0.6,-0.584615384615384,-0.569230769230769,
-0.553846153846154,-0.538461538461538,-0.523076923076923,-0.507692307692308,
-0.492307692307692,-0.476923076923077,-0.461538461538462,-0.446153846153846,
-0.430769230769231,-0.415384615384615,-0.4,-0.384615384615385,-0.369230769230769,
-0.353846153846154,-0.338461538461538,-0.323076923076923,-0.307692307692308,
-0.292307692307692,-0.276923076923077,-0.261538461538462,-0.246153846153846,
-0.230769230769231,-0.215384615384615,-0.2,-0.184615384615385,-0.169230769230769,
-0.153846153846154,-0.138461538461538,-0.123076923076923,-0.107692307692308,
-0.0923076923076923,-0.0769230769230769,-0.0615384615384615,-0.0461538461538462,
-0.0307692307692308,-0.0153846153846154,0.),.UNSPECIFIED.)
CURVE()
GEOMETRIC_REPRESENTATION_ITEM()
RATIONAL_B_SPLINE_CURVE((1.,1.,1.,1.,1.,1.,1.,1.,1.,1.,1.,1.,1.,1.,1.,1.,
1.,1.,1.,1.,1.,1.,1.,1.,1.,1.,1.,1.,1.,1.,1.,1.,1.,1.,1.,1.,1.,1.,1.,1.,
1.,1.,1.,1.,1.,1.,1.,1.,1.,1.,1.,1.,1.,1.,1.,1.,1.,1.,1.,1.,1.,1.,1.,1.,
1.,1.,1.,1.,1.,1.))
REPRESENTATION_ITEM('')
);
#109=(
BOUNDED_CURVE()
B_SPLINE_CURVE(5,(#27805,#27806,#27807,#27808,#27809,#27810,#27811,#27812,
#27813,#27814,#27815,#27816,#27817,#27818,#27819,#27820,#27821,#27822,#27823,
#27824,#27825,#27826,#27827,#27828,#27829,#27830,#27831,#27832,#27833,#27834,
#27835,#27836,#27837,#27838,#27839,#27840,#27841,#27842,#27843,#27844,#27845,
#27846,#27847,#27848,#27849,#27850,#27851,#27852,#27853,#27854,#27855,#27856,
#27857,#27858,#27859,#27860,#27861,#27862,#27863,#27864,#27865,#27866,#27867,
#27868,#27869,#27870,#27871,#27872,#27873,#27874),.UNSPECIFIED.,.F.,.F.)
B_SPLINE_CURVE_WITH_KNOTS((6,1,1,1,1,1,1,1,1,1,1,1,1,1,1,1,1,1,1,1,1,1,
1,1,1,1,1,1,1,1,1,1,1,1,1,1,1,1,1,1,1,1,1,1,1,1,1,1,1,1,1,1,1,1,1,1,1,1,
1,1,1,1,1,1,1,6),(-1.,-0.984615384615383,-0.969230769230768,-0.953846153846152,
-0.938461538461537,-0.923076923076922,-0.907692307692306,-0.892307692307691,
-0.876923076923076,-0.86153846153846,-0.846153846153845,-0.83076923076923,
-0.815384615384614,-0.799999999999999,-0.784615384615384,-0.769230769230768,
-0.753846153846153,-0.738461538461538,-0.723076923076922,-0.707692307692307,
-0.692307692307692,-0.676923076923076,-0.661538461538461,-0.646153846153846,
-0.63076923076923,-0.615384615384615,-0.6,-0.584615384615384,-0.569230769230769,
-0.553846153846154,-0.538461538461538,-0.523076923076923,-0.507692307692308,
-0.492307692307692,-0.476923076923077,-0.461538461538462,-0.446153846153846,
-0.430769230769231,-0.415384615384615,-0.4,-0.384615384615385,-0.369230769230769,
-0.353846153846154,-0.338461538461538,-0.323076923076923,-0.307692307692308,
-0.292307692307692,-0.276923076923077,-0.261538461538462,-0.246153846153846,
-0.230769230769231,-0.215384615384615,-0.2,-0.184615384615385,-0.169230769230769,
-0.153846153846154,-0.138461538461538,-0.123076923076923,-0.107692307692308,
-0.0923076923076923,-0.0769230769230769,-0.0615384615384615,-0.0461538461538462,
-0.0307692307692308,-0.0153846153846154,0.),.UNSPECIFIED.)
CURVE()
GEOMETRIC_REPRESENTATION_ITEM()
RATIONAL_B_SPLINE_CURVE((1.,1.,1.,1.,1.,1.,1.,1.,1.,1.,1.,1.,1.,1.,1.,1.,
1.,1.,1.,1.,1.,1.,1.,1.,1.,1.,1.,1.,1.,1.,1.,1.,1.,1.,1.,1.,1.,1.,1.,1.,
1.,1.,1.,1.,1.,1.,1.,1.,1.,1.,1.,1.,1.,1.,1.,1.,1.,1.,1.,1.,1.,1.,1.,1.,
1.,1.,1.,1.,1.,1.))
REPRESENTATION_ITEM('')
);
#110=(
BOUNDED_CURVE()
B_SPLINE_CURVE(5,(#28021,#28022,#28023,#28024,#28025,#28026,#28027,#28028,
#28029,#28030,#28031,#28032,#28033,#28034,#28035,#28036,#28037,#28038,#28039,
#28040,#28041,#28042,#28043,#28044,#28045,#28046,#28047,#28048,#28049,#28050,
#28051,#28052,#28053,#28054,#28055,#28056,#28057,#28058,#28059,#28060,#28061,
#28062,#28063,#28064,#28065,#28066,#28067,#28068,#28069,#28070,#28071,#28072,
#28073,#28074,#28075,#28076,#28077,#28078,#28079,#28080,#28081,#28082,#28083,
#28084,#28085,#28086,#28087,#28088,#28089,#28090),.UNSPECIFIED.,.F.,.F.)
B_SPLINE_CURVE_WITH_KNOTS((6,1,1,1,1,1,1,1,1,1,1,1,1,1,1,1,1,1,1,1,1,1,
1,1,1,1,1,1,1,1,1,1,1,1,1,1,1,1,1,1,1,1,1,1,1,1,1,1,1,1,1,1,1,1,1,1,1,1,
1,1,1,1,1,1,1,6),(-1.,-0.984615384615383,-0.969230769230768,-0.953846153846152,
-0.938461538461537,-0.923076923076922,-0.907692307692306,-0.892307692307691,
-0.876923076923076,-0.86153846153846,-0.846153846153845,-0.83076923076923,
-0.815384615384614,-0.799999999999999,-0.784615384615384,-0.769230769230768,
-0.753846153846153,-0.738461538461538,-0.723076923076922,-0.707692307692307,
-0.692307692307692,-0.676923076923076,-0.661538461538461,-0.646153846153846,
-0.63076923076923,-0.615384615384615,-0.6,-0.584615384615384,-0.569230769230769,
-0.553846153846154,-0.538461538461538,-0.523076923076923,-0.507692307692308,
-0.492307692307692,-0.476923076923077,-0.461538461538462,-0.446153846153846,
-0.430769230769231,-0.415384615384615,-0.4,-0.384615384615385,-0.369230769230769,
-0.353846153846154,-0.338461538461538,-0.323076923076923,-0.307692307692308,
-0.292307692307692,-0.276923076923077,-0.261538461538462,-0.246153846153846,
-0.230769230769231,-0.215384615384615,-0.2,-0.184615384615385,-0.169230769230769,
-0.153846153846154,-0.138461538461538,-0.123076923076923,-0.107692307692308,
-0.0923076923076923,-0.0769230769230769,-0.0615384615384615,-0.0461538461538462,
-0.0307692307692308,-0.0153846153846154,0.),.UNSPECIFIED.)
CURVE()
GEOMETRIC_REPRESENTATION_ITEM()
RATIONAL_B_SPLINE_CURVE((1.,1.,1.,1.,1.,1.,1.,1.,1.,1.,1.,1.,1.,1.,1.,1.,
1.,1.,1.,1.,1.,1.,1.,1.,1.,1.,1.,1.,1.,1.,1.,1.,1.,1.,1.,1.,1.,1.,1.,1.,
1.,1.,1.,1.,1.,1.,1.,1.,1.,1.,1.,1.,1.,1.,1.,1.,1.,1.,1.,1.,1.,1.,1.,1.,
1.,1.,1.,1.,1.,1.))
REPRESENTATION_ITEM('')
);
#111=(
BOUNDED_CURVE()
B_SPLINE_CURVE(5,(#28237,#28238,#28239,#28240,#28241,#28242,#28243,#28244,
#28245,#28246,#28247,#28248,#28249,#28250,#28251,#28252,#28253,#28254,#28255,
#28256,#28257,#28258,#28259,#28260,#28261,#28262,#28263,#28264,#28265,#28266,
#28267,#28268,#28269,#28270,#28271,#28272,#28273,#28274,#28275,#28276,#28277,
#28278,#28279,#28280,#28281,#28282,#28283,#28284,#28285,#28286,#28287,#28288,
#28289,#28290,#28291,#28292,#28293,#28294,#28295,#28296,#28297,#28298,#28299,
#28300,#28301,#28302,#28303,#28304,#28305,#28306),.UNSPECIFIED.,.F.,.F.)
B_SPLINE_CURVE_WITH_KNOTS((6,1,1,1,1,1,1,1,1,1,1,1,1,1,1,1,1,1,1,1,1,1,
1,1,1,1,1,1,1,1,1,1,1,1,1,1,1,1,1,1,1,1,1,1,1,1,1,1,1,1,1,1,1,1,1,1,1,1,
1,1,1,1,1,1,1,6),(-1.,-0.984615384615383,-0.969230769230768,-0.953846153846152,
-0.938461538461537,-0.923076923076922,-0.907692307692306,-0.892307692307691,
-0.876923076923076,-0.86153846153846,-0.846153846153845,-0.83076923076923,
-0.815384615384614,-0.799999999999999,-0.784615384615384,-0.769230769230768,
-0.753846153846153,-0.738461538461538,-0.723076923076922,-0.707692307692307,
-0.692307692307692,-0.676923076923076,-0.661538461538461,-0.646153846153846,
-0.63076923076923,-0.615384615384615,-0.6,-0.584615384615384,-0.569230769230769,
-0.553846153846154,-0.538461538461538,-0.523076923076923,-0.507692307692308,
-0.492307692307692,-0.476923076923077,-0.461538461538462,-0.446153846153846,
-0.430769230769231,-0.415384615384615,-0.4,-0.384615384615385,-0.369230769230769,
-0.353846153846154,-0.338461538461538,-0.323076923076923,-0.307692307692308,
-0.292307692307692,-0.276923076923077,-0.261538461538462,-0.246153846153846,
-0.230769230769231,-0.215384615384615,-0.2,-0.184615384615385,-0.169230769230769,
-0.153846153846154,-0.138461538461538,-0.123076923076923,-0.107692307692308,
-0.0923076923076923,-0.0769230769230769,-0.0615384615384615,-0.0461538461538462,
-0.0307692307692308,-0.0153846153846154,0.),.UNSPECIFIED.)
CURVE()
GEOMETRIC_REPRESENTATION_ITEM()
RATIONAL_B_SPLINE_CURVE((1.,1.,1.,1.,1.,1.,1.,1.,1.,1.,1.,1.,1.,1.,1.,1.,
1.,1.,1.,1.,1.,1.,1.,1.,1.,1.,1.,1.,1.,1.,1.,1.,1.,1.,1.,1.,1.,1.,1.,1.,
1.,1.,1.,1.,1.,1.,1.,1.,1.,1.,1.,1.,1.,1.,1.,1.,1.,1.,1.,1.,1.,1.,1.,1.,
1.,1.,1.,1.,1.,1.))
REPRESENTATION_ITEM('')
);
#112=(
BOUNDED_CURVE()
B_SPLINE_CURVE(5,(#28453,#28454,#28455,#28456,#28457,#28458,#28459,#28460,
#28461,#28462,#28463,#28464,#28465,#28466,#28467,#28468,#28469,#28470,#28471,
#28472,#28473,#28474,#28475,#28476,#28477,#28478,#28479,#28480,#28481,#28482,
#28483,#28484,#28485,#28486,#28487,#28488,#28489,#28490,#28491,#28492,#28493,
#28494,#28495,#28496,#28497,#28498,#28499,#28500,#28501,#28502,#28503,#28504,
#28505,#28506,#28507,#28508,#28509,#28510,#28511,#28512,#28513,#28514,#28515,
#28516,#28517,#28518,#28519,#28520,#28521,#28522),.UNSPECIFIED.,.F.,.F.)
B_SPLINE_CURVE_WITH_KNOTS((6,1,1,1,1,1,1,1,1,1,1,1,1,1,1,1,1,1,1,1,1,1,
1,1,1,1,1,1,1,1,1,1,1,1,1,1,1,1,1,1,1,1,1,1,1,1,1,1,1,1,1,1,1,1,1,1,1,1,
1,1,1,1,1,1,1,6),(-1.,-0.984615384615383,-0.969230769230768,-0.953846153846152,
-0.938461538461537,-0.923076923076922,-0.907692307692306,-0.892307692307691,
-0.876923076923076,-0.86153846153846,-0.846153846153845,-0.83076923076923,
-0.815384615384614,-0.799999999999999,-0.784615384615384,-0.769230769230768,
-0.753846153846153,-0.738461538461538,-0.723076923076922,-0.707692307692307,
-0.692307692307692,-0.676923076923076,-0.661538461538461,-0.646153846153846,
-0.63076923076923,-0.615384615384615,-0.6,-0.584615384615384,-0.569230769230769,
-0.553846153846154,-0.538461538461538,-0.523076923076923,-0.507692307692308,
-0.492307692307692,-0.476923076923077,-0.461538461538462,-0.446153846153846,
-0.430769230769231,-0.415384615384615,-0.4,-0.384615384615385,-0.369230769230769,
-0.353846153846154,-0.338461538461538,-0.323076923076923,-0.307692307692308,
-0.292307692307692,-0.276923076923077,-0.261538461538462,-0.246153846153846,
-0.230769230769231,-0.215384615384615,-0.2,-0.184615384615385,-0.169230769230769,
-0.153846153846154,-0.138461538461538,-0.123076923076923,-0.107692307692308,
-0.0923076923076923,-0.0769230769230769,-0.0615384615384615,-0.0461538461538462,
-0.0307692307692308,-0.0153846153846154,0.),.UNSPECIFIED.)
CURVE()
GEOMETRIC_REPRESENTATION_ITEM()
RATIONAL_B_SPLINE_CURVE((1.,1.,1.,1.,1.,1.,1.,1.,1.,1.,1.,1.,1.,1.,1.,1.,
1.,1.,1.,1.,1.,1.,1.,1.,1.,1.,1.,1.,1.,1.,1.,1.,1.,1.,1.,1.,1.,1.,1.,1.,
1.,1.,1.,1.,1.,1.,1.,1.,1.,1.,1.,1.,1.,1.,1.,1.,1.,1.,1.,1.,1.,1.,1.,1.,
1.,1.,1.,1.,1.,1.))
REPRESENTATION_ITEM('')
);
#113=(
BOUNDED_CURVE()
B_SPLINE_CURVE(5,(#28669,#28670,#28671,#28672,#28673,#28674,#28675,#28676,
#28677,#28678,#28679,#28680,#28681,#28682,#28683,#28684,#28685,#28686,#28687,
#28688,#28689,#28690,#28691,#28692,#28693,#28694,#28695,#28696,#28697,#28698,
#28699,#28700,#28701,#28702,#28703,#28704,#28705,#28706,#28707,#28708,#28709,
#28710,#28711,#28712,#28713,#28714,#28715,#28716,#28717,#28718,#28719,#28720,
#28721,#28722,#28723,#28724,#28725,#28726,#28727,#28728,#28729,#28730,#28731,
#28732,#28733,#28734,#28735,#28736,#28737,#28738),.UNSPECIFIED.,.F.,.F.)
B_SPLINE_CURVE_WITH_KNOTS((6,1,1,1,1,1,1,1,1,1,1,1,1,1,1,1,1,1,1,1,1,1,
1,1,1,1,1,1,1,1,1,1,1,1,1,1,1,1,1,1,1,1,1,1,1,1,1,1,1,1,1,1,1,1,1,1,1,1,
1,1,1,1,1,1,1,6),(-1.,-0.984615384615383,-0.969230769230768,-0.953846153846152,
-0.938461538461537,-0.923076923076922,-0.907692307692306,-0.892307692307691,
-0.876923076923076,-0.86153846153846,-0.846153846153845,-0.83076923076923,
-0.815384615384614,-0.799999999999999,-0.784615384615384,-0.769230769230768,
-0.753846153846153,-0.738461538461538,-0.723076923076922,-0.707692307692307,
-0.692307692307692,-0.676923076923076,-0.661538461538461,-0.646153846153846,
-0.63076923076923,-0.615384615384615,-0.6,-0.584615384615384,-0.569230769230769,
-0.553846153846154,-0.538461538461538,-0.523076923076923,-0.507692307692308,
-0.492307692307692,-0.476923076923077,-0.461538461538462,-0.446153846153846,
-0.430769230769231,-0.415384615384615,-0.4,-0.384615384615385,-0.369230769230769,
-0.353846153846154,-0.338461538461538,-0.323076923076923,-0.307692307692308,
-0.292307692307692,-0.276923076923077,-0.261538461538462,-0.246153846153846,
-0.230769230769231,-0.215384615384615,-0.2,-0.184615384615385,-0.169230769230769,
-0.153846153846154,-0.138461538461538,-0.123076923076923,-0.107692307692308,
-0.0923076923076923,-0.0769230769230769,-0.0615384615384615,-0.0461538461538462,
-0.0307692307692308,-0.0153846153846154,0.),.UNSPECIFIED.)
CURVE()
GEOMETRIC_REPRESENTATION_ITEM()
RATIONAL_B_SPLINE_CURVE((1.,1.,1.,1.,1.,1.,1.,1.,1.,1.,1.,1.,1.,1.,1.,1.,
1.,1.,1.,1.,1.,1.,1.,1.,1.,1.,1.,1.,1.,1.,1.,1.,1.,1.,1.,1.,1.,1.,1.,1.,
1.,1.,1.,1.,1.,1.,1.,1.,1.,1.,1.,1.,1.,1.,1.,1.,1.,1.,1.,1.,1.,1.,1.,1.,
1.,1.,1.,1.,1.,1.))
REPRESENTATION_ITEM('')
);
#114=(
BOUNDED_CURVE()
B_SPLINE_CURVE(5,(#28885,#28886,#28887,#28888,#28889,#28890,#28891,#28892,
#28893,#28894,#28895,#28896,#28897,#28898,#28899,#28900,#28901,#28902,#28903,
#28904,#28905,#28906,#28907,#28908,#28909,#28910,#28911,#28912,#28913,#28914,
#28915,#28916,#28917,#28918,#28919,#28920,#28921,#28922,#28923,#28924,#28925,
#28926,#28927,#28928,#28929,#28930,#28931,#28932,#28933,#28934,#28935,#28936,
#28937,#28938,#28939,#28940,#28941,#28942,#28943,#28944,#28945,#28946,#28947,
#28948,#28949,#28950,#28951,#28952,#28953,#28954),.UNSPECIFIED.,.F.,.F.)
B_SPLINE_CURVE_WITH_KNOTS((6,1,1,1,1,1,1,1,1,1,1,1,1,1,1,1,1,1,1,1,1,1,
1,1,1,1,1,1,1,1,1,1,1,1,1,1,1,1,1,1,1,1,1,1,1,1,1,1,1,1,1,1,1,1,1,1,1,1,
1,1,1,1,1,1,1,6),(-1.,-0.984615384615383,-0.969230769230768,-0.953846153846152,
-0.938461538461537,-0.923076923076922,-0.907692307692306,-0.892307692307691,
-0.876923076923076,-0.86153846153846,-0.846153846153845,-0.83076923076923,
-0.815384615384614,-0.799999999999999,-0.784615384615384,-0.769230769230768,
-0.753846153846153,-0.738461538461538,-0.723076923076922,-0.707692307692307,
-0.692307692307692,-0.676923076923076,-0.661538461538461,-0.646153846153846,
-0.63076923076923,-0.615384615384615,-0.6,-0.584615384615384,-0.569230769230769,
-0.553846153846154,-0.538461538461538,-0.523076923076923,-0.507692307692308,
-0.492307692307692,-0.476923076923077,-0.461538461538462,-0.446153846153846,
-0.430769230769231,-0.415384615384615,-0.4,-0.384615384615385,-0.369230769230769,
-0.353846153846154,-0.338461538461538,-0.323076923076923,-0.307692307692308,
-0.292307692307692,-0.276923076923077,-0.261538461538462,-0.246153846153846,
-0.230769230769231,-0.215384615384615,-0.2,-0.184615384615385,-0.169230769230769,
-0.153846153846154,-0.138461538461538,-0.123076923076923,-0.107692307692308,
-0.0923076923076923,-0.0769230769230769,-0.0615384615384615,-0.0461538461538462,
-0.0307692307692308,-0.0153846153846154,0.),.UNSPECIFIED.)
CURVE()
GEOMETRIC_REPRESENTATION_ITEM()
RATIONAL_B_SPLINE_CURVE((1.,1.,1.,1.,1.,1.,1.,1.,1.,1.,1.,1.,1.,1.,1.,1.,
1.,1.,1.,1.,1.,1.,1.,1.,1.,1.,1.,1.,1.,1.,1.,1.,1.,1.,1.,1.,1.,1.,1.,1.,
1.,1.,1.,1.,1.,1.,1.,1.,1.,1.,1.,1.,1.,1.,1.,1.,1.,1.,1.,1.,1.,1.,1.,1.,
1.,1.,1.,1.,1.,1.))
REPRESENTATION_ITEM('')
);
#115=(
BOUNDED_CURVE()
B_SPLINE_CURVE(5,(#29101,#29102,#29103,#29104,#29105,#29106,#29107,#29108,
#29109,#29110,#29111,#29112,#29113,#29114,#29115,#29116,#29117,#29118,#29119,
#29120,#29121,#29122,#29123,#29124,#29125,#29126,#29127,#29128,#29129,#29130,
#29131,#29132,#29133,#29134,#29135,#29136,#29137,#29138,#29139,#29140,#29141,
#29142,#29143,#29144,#29145,#29146,#29147,#29148,#29149,#29150,#29151,#29152,
#29153,#29154,#29155,#29156,#29157,#29158,#29159,#29160,#29161,#29162,#29163,
#29164,#29165,#29166,#29167,#29168,#29169,#29170),.UNSPECIFIED.,.F.,.F.)
B_SPLINE_CURVE_WITH_KNOTS((6,1,1,1,1,1,1,1,1,1,1,1,1,1,1,1,1,1,1,1,1,1,
1,1,1,1,1,1,1,1,1,1,1,1,1,1,1,1,1,1,1,1,1,1,1,1,1,1,1,1,1,1,1,1,1,1,1,1,
1,1,1,1,1,1,1,6),(-1.,-0.984615384615383,-0.969230769230768,-0.953846153846152,
-0.938461538461537,-0.923076923076922,-0.907692307692306,-0.892307692307691,
-0.876923076923076,-0.86153846153846,-0.846153846153845,-0.83076923076923,
-0.815384615384614,-0.799999999999999,-0.784615384615384,-0.769230769230768,
-0.753846153846153,-0.738461538461538,-0.723076923076922,-0.707692307692307,
-0.692307692307692,-0.676923076923076,-0.661538461538461,-0.646153846153846,
-0.63076923076923,-0.615384615384615,-0.6,-0.584615384615384,-0.569230769230769,
-0.553846153846154,-0.538461538461538,-0.523076923076923,-0.507692307692308,
-0.492307692307692,-0.476923076923077,-0.461538461538462,-0.446153846153846,
-0.430769230769231,-0.415384615384615,-0.4,-0.384615384615385,-0.369230769230769,
-0.353846153846154,-0.338461538461538,-0.323076923076923,-0.307692307692308,
-0.292307692307692,-0.276923076923077,-0.261538461538462,-0.246153846153846,
-0.230769230769231,-0.215384615384615,-0.2,-0.184615384615385,-0.169230769230769,
-0.153846153846154,-0.138461538461538,-0.123076923076923,-0.107692307692308,
-0.0923076923076923,-0.0769230769230769,-0.0615384615384615,-0.0461538461538462,
-0.0307692307692308,-0.0153846153846154,0.),.UNSPECIFIED.)
CURVE()
GEOMETRIC_REPRESENTATION_ITEM()
RATIONAL_B_SPLINE_CURVE((1.,1.,1.,1.,1.,1.,1.,1.,1.,1.,1.,1.,1.,1.,1.,1.,
1.,1.,1.,1.,1.,1.,1.,1.,1.,1.,1.,1.,1.,1.,1.,1.,1.,1.,1.,1.,1.,1.,1.,1.,
1.,1.,1.,1.,1.,1.,1.,1.,1.,1.,1.,1.,1.,1.,1.,1.,1.,1.,1.,1.,1.,1.,1.,1.,
1.,1.,1.,1.,1.,1.))
REPRESENTATION_ITEM('')
);
#116=(
BOUNDED_CURVE()
B_SPLINE_CURVE(5,(#29317,#29318,#29319,#29320,#29321,#29322,#29323,#29324,
#29325,#29326,#29327,#29328,#29329,#29330,#29331,#29332,#29333,#29334,#29335,
#29336,#29337,#29338,#29339,#29340,#29341,#29342,#29343,#29344,#29345,#29346,
#29347,#29348,#29349,#29350,#29351,#29352,#29353,#29354,#29355,#29356,#29357,
#29358,#29359,#29360,#29361,#29362,#29363,#29364,#29365,#29366,#29367,#29368,
#29369,#29370,#29371,#29372,#29373,#29374,#29375,#29376,#29377,#29378,#29379,
#29380,#29381,#29382,#29383,#29384,#29385,#29386),.UNSPECIFIED.,.F.,.F.)
B_SPLINE_CURVE_WITH_KNOTS((6,1,1,1,1,1,1,1,1,1,1,1,1,1,1,1,1,1,1,1,1,1,
1,1,1,1,1,1,1,1,1,1,1,1,1,1,1,1,1,1,1,1,1,1,1,1,1,1,1,1,1,1,1,1,1,1,1,1,
1,1,1,1,1,1,1,6),(-1.,-0.984615384615383,-0.969230769230768,-0.953846153846152,
-0.938461538461537,-0.923076923076922,-0.907692307692306,-0.892307692307691,
-0.876923076923076,-0.86153846153846,-0.846153846153845,-0.83076923076923,
-0.815384615384614,-0.799999999999999,-0.784615384615384,-0.769230769230768,
-0.753846153846153,-0.738461538461538,-0.723076923076922,-0.707692307692307,
-0.692307692307692,-0.676923076923076,-0.661538461538461,-0.646153846153846,
-0.63076923076923,-0.615384615384615,-0.6,-0.584615384615384,-0.569230769230769,
-0.553846153846154,-0.538461538461538,-0.523076923076923,-0.507692307692308,
-0.492307692307692,-0.476923076923077,-0.461538461538462,-0.446153846153846,
-0.430769230769231,-0.415384615384615,-0.4,-0.384615384615385,-0.369230769230769,
-0.353846153846154,-0.338461538461538,-0.323076923076923,-0.307692307692308,
-0.292307692307692,-0.276923076923077,-0.261538461538462,-0.246153846153846,
-0.230769230769231,-0.215384615384615,-0.2,-0.184615384615385,-0.169230769230769,
-0.153846153846154,-0.138461538461538,-0.123076923076923,-0.107692307692308,
-0.0923076923076923,-0.0769230769230769,-0.0615384615384615,-0.0461538461538462,
-0.0307692307692308,-0.0153846153846154,0.),.UNSPECIFIED.)
CURVE()
GEOMETRIC_REPRESENTATION_ITEM()
RATIONAL_B_SPLINE_CURVE((1.,1.,1.,1.,1.,1.,1.,1.,1.,1.,1.,1.,1.,1.,1.,1.,
1.,1.,1.,1.,1.,1.,1.,1.,1.,1.,1.,1.,1.,1.,1.,1.,1.,1.,1.,1.,1.,1.,1.,1.,
1.,1.,1.,1.,1.,1.,1.,1.,1.,1.,1.,1.,1.,1.,1.,1.,1.,1.,1.,1.,1.,1.,1.,1.,
1.,1.,1.,1.,1.,1.))
REPRESENTATION_ITEM('')
);
#117=(
BOUNDED_CURVE()
B_SPLINE_CURVE(5,(#29533,#29534,#29535,#29536,#29537,#29538,#29539,#29540,
#29541,#29542,#29543,#29544,#29545,#29546,#29547,#29548,#29549,#29550,#29551,
#29552,#29553,#29554,#29555,#29556,#29557,#29558,#29559,#29560,#29561,#29562,
#29563,#29564,#29565,#29566,#29567,#29568,#29569,#29570,#29571,#29572,#29573,
#29574,#29575,#29576,#29577,#29578,#29579,#29580,#29581,#29582,#29583,#29584,
#29585,#29586,#29587,#29588,#29589,#29590,#29591,#29592,#29593,#29594,#29595,
#29596,#29597,#29598,#29599,#29600,#29601,#29602),.UNSPECIFIED.,.F.,.F.)
B_SPLINE_CURVE_WITH_KNOTS((6,1,1,1,1,1,1,1,1,1,1,1,1,1,1,1,1,1,1,1,1,1,
1,1,1,1,1,1,1,1,1,1,1,1,1,1,1,1,1,1,1,1,1,1,1,1,1,1,1,1,1,1,1,1,1,1,1,1,
1,1,1,1,1,1,1,6),(-1.,-0.984615384615383,-0.969230769230768,-0.953846153846152,
-0.938461538461537,-0.923076923076922,-0.907692307692306,-0.892307692307691,
-0.876923076923076,-0.86153846153846,-0.846153846153845,-0.83076923076923,
-0.815384615384614,-0.799999999999999,-0.784615384615384,-0.769230769230768,
-0.753846153846153,-0.738461538461538,-0.723076923076922,-0.707692307692307,
-0.692307692307692,-0.676923076923076,-0.661538461538461,-0.646153846153846,
-0.63076923076923,-0.615384615384615,-0.6,-0.584615384615384,-0.569230769230769,
-0.553846153846154,-0.538461538461538,-0.523076923076923,-0.507692307692308,
-0.492307692307692,-0.476923076923077,-0.461538461538462,-0.446153846153846,
-0.430769230769231,-0.415384615384615,-0.4,-0.384615384615385,-0.369230769230769,
-0.353846153846154,-0.338461538461538,-0.323076923076923,-0.307692307692308,
-0.292307692307692,-0.276923076923077,-0.261538461538462,-0.246153846153846,
-0.230769230769231,-0.215384615384615,-0.2,-0.184615384615385,-0.169230769230769,
-0.153846153846154,-0.138461538461538,-0.123076923076923,-0.107692307692308,
-0.0923076923076923,-0.0769230769230769,-0.0615384615384615,-0.0461538461538462,
-0.0307692307692308,-0.0153846153846154,0.),.UNSPECIFIED.)
CURVE()
GEOMETRIC_REPRESENTATION_ITEM()
RATIONAL_B_SPLINE_CURVE((1.,1.,1.,1.,1.,1.,1.,1.,1.,1.,1.,1.,1.,1.,1.,1.,
1.,1.,1.,1.,1.,1.,1.,1.,1.,1.,1.,1.,1.,1.,1.,1.,1.,1.,1.,1.,1.,1.,1.,1.,
1.,1.,1.,1.,1.,1.,1.,1.,1.,1.,1.,1.,1.,1.,1.,1.,1.,1.,1.,1.,1.,1.,1.,1.,
1.,1.,1.,1.,1.,1.))
REPRESENTATION_ITEM('')
);
#118=(
BOUNDED_CURVE()
B_SPLINE_CURVE(5,(#29749,#29750,#29751,#29752,#29753,#29754,#29755,#29756,
#29757,#29758,#29759,#29760,#29761,#29762,#29763,#29764,#29765,#29766,#29767,
#29768,#29769,#29770,#29771,#29772,#29773,#29774,#29775,#29776,#29777,#29778,
#29779,#29780,#29781,#29782,#29783,#29784,#29785,#29786,#29787,#29788,#29789,
#29790,#29791,#29792,#29793,#29794,#29795,#29796,#29797,#29798,#29799,#29800,
#29801,#29802,#29803,#29804,#29805,#29806,#29807,#29808,#29809,#29810,#29811,
#29812,#29813,#29814,#29815,#29816,#29817,#29818),.UNSPECIFIED.,.F.,.F.)
B_SPLINE_CURVE_WITH_KNOTS((6,1,1,1,1,1,1,1,1,1,1,1,1,1,1,1,1,1,1,1,1,1,
1,1,1,1,1,1,1,1,1,1,1,1,1,1,1,1,1,1,1,1,1,1,1,1,1,1,1,1,1,1,1,1,1,1,1,1,
1,1,1,1,1,1,1,6),(-1.,-0.984615384615383,-0.969230769230768,-0.953846153846152,
-0.938461538461537,-0.923076923076922,-0.907692307692306,-0.892307692307691,
-0.876923076923076,-0.86153846153846,-0.846153846153845,-0.83076923076923,
-0.815384615384614,-0.799999999999999,-0.784615384615384,-0.769230769230768,
-0.753846153846153,-0.738461538461538,-0.723076923076922,-0.707692307692307,
-0.692307692307692,-0.676923076923076,-0.661538461538461,-0.646153846153846,
-0.63076923076923,-0.615384615384615,-0.6,-0.584615384615384,-0.569230769230769,
-0.553846153846154,-0.538461538461538,-0.523076923076923,-0.507692307692308,
-0.492307692307692,-0.476923076923077,-0.461538461538462,-0.446153846153846,
-0.430769230769231,-0.415384615384615,-0.4,-0.384615384615385,-0.369230769230769,
-0.353846153846154,-0.338461538461538,-0.323076923076923,-0.307692307692308,
-0.292307692307692,-0.276923076923077,-0.261538461538462,-0.246153846153846,
-0.230769230769231,-0.215384615384615,-0.2,-0.184615384615385,-0.169230769230769,
-0.153846153846154,-0.138461538461538,-0.123076923076923,-0.107692307692308,
-0.0923076923076923,-0.0769230769230769,-0.0615384615384615,-0.0461538461538462,
-0.0307692307692308,-0.0153846153846154,0.),.UNSPECIFIED.)
CURVE()
GEOMETRIC_REPRESENTATION_ITEM()
RATIONAL_B_SPLINE_CURVE((1.,1.,1.,1.,1.,1.,1.,1.,1.,1.,1.,1.,1.,1.,1.,1.,
1.,1.,1.,1.,1.,1.,1.,1.,1.,1.,1.,1.,1.,1.,1.,1.,1.,1.,1.,1.,1.,1.,1.,1.,
1.,1.,1.,1.,1.,1.,1.,1.,1.,1.,1.,1.,1.,1.,1.,1.,1.,1.,1.,1.,1.,1.,1.,1.,
1.,1.,1.,1.,1.,1.))
REPRESENTATION_ITEM('')
);
#119=(
BOUNDED_CURVE()
B_SPLINE_CURVE(5,(#29965,#29966,#29967,#29968,#29969,#29970,#29971,#29972,
#29973,#29974,#29975,#29976,#29977,#29978,#29979,#29980,#29981,#29982,#29983,
#29984,#29985,#29986,#29987,#29988,#29989,#29990,#29991,#29992,#29993,#29994,
#29995,#29996,#29997,#29998,#29999,#30000,#30001,#30002,#30003,#30004,#30005,
#30006,#30007,#30008,#30009,#30010,#30011,#30012,#30013,#30014,#30015,#30016,
#30017,#30018,#30019,#30020,#30021,#30022,#30023,#30024,#30025,#30026,#30027,
#30028,#30029,#30030,#30031,#30032,#30033,#30034),.UNSPECIFIED.,.F.,.F.)
B_SPLINE_CURVE_WITH_KNOTS((6,1,1,1,1,1,1,1,1,1,1,1,1,1,1,1,1,1,1,1,1,1,
1,1,1,1,1,1,1,1,1,1,1,1,1,1,1,1,1,1,1,1,1,1,1,1,1,1,1,1,1,1,1,1,1,1,1,1,
1,1,1,1,1,1,1,6),(-1.,-0.984615384615383,-0.969230769230768,-0.953846153846152,
-0.938461538461537,-0.923076923076922,-0.907692307692306,-0.892307692307691,
-0.876923076923076,-0.86153846153846,-0.846153846153845,-0.83076923076923,
-0.815384615384614,-0.799999999999999,-0.784615384615384,-0.769230769230768,
-0.753846153846153,-0.738461538461538,-0.723076923076922,-0.707692307692307,
-0.692307692307692,-0.676923076923076,-0.661538461538461,-0.646153846153846,
-0.63076923076923,-0.615384615384615,-0.6,-0.584615384615384,-0.569230769230769,
-0.553846153846154,-0.538461538461538,-0.523076923076923,-0.507692307692308,
-0.492307692307692,-0.476923076923077,-0.461538461538462,-0.446153846153846,
-0.430769230769231,-0.415384615384615,-0.4,-0.384615384615385,-0.369230769230769,
-0.353846153846154,-0.338461538461538,-0.323076923076923,-0.307692307692308,
-0.292307692307692,-0.276923076923077,-0.261538461538462,-0.246153846153846,
-0.230769230769231,-0.215384615384615,-0.2,-0.184615384615385,-0.169230769230769,
-0.153846153846154,-0.138461538461538,-0.123076923076923,-0.107692307692308,
-0.0923076923076923,-0.0769230769230769,-0.0615384615384615,-0.0461538461538462,
-0.0307692307692308,-0.0153846153846154,0.),.UNSPECIFIED.)
CURVE()
GEOMETRIC_REPRESENTATION_ITEM()
RATIONAL_B_SPLINE_CURVE((1.,1.,1.,1.,1.,1.,1.,1.,1.,1.,1.,1.,1.,1.,1.,1.,
1.,1.,1.,1.,1.,1.,1.,1.,1.,1.,1.,1.,1.,1.,1.,1.,1.,1.,1.,1.,1.,1.,1.,1.,
1.,1.,1.,1.,1.,1.,1.,1.,1.,1.,1.,1.,1.,1.,1.,1.,1.,1.,1.,1.,1.,1.,1.,1.,
1.,1.,1.,1.,1.,1.))
REPRESENTATION_ITEM('')
);
#120=(
BOUNDED_CURVE()
B_SPLINE_CURVE(5,(#30181,#30182,#30183,#30184,#30185,#30186,#30187,#30188,
#30189,#30190,#30191,#30192,#30193,#30194,#30195,#30196,#30197,#30198,#30199,
#30200,#30201,#30202,#30203,#30204,#30205,#30206,#30207,#30208,#30209,#30210,
#30211,#30212,#30213,#30214,#30215,#30216,#30217,#30218,#30219,#30220,#30221,
#30222,#30223,#30224,#30225,#30226,#30227,#30228,#30229,#30230,#30231,#30232,
#30233,#30234,#30235,#30236,#30237,#30238,#30239,#30240,#30241,#30242,#30243,
#30244,#30245,#30246,#30247,#30248,#30249,#30250),.UNSPECIFIED.,.F.,.F.)
B_SPLINE_CURVE_WITH_KNOTS((6,1,1,1,1,1,1,1,1,1,1,1,1,1,1,1,1,1,1,1,1,1,
1,1,1,1,1,1,1,1,1,1,1,1,1,1,1,1,1,1,1,1,1,1,1,1,1,1,1,1,1,1,1,1,1,1,1,1,
1,1,1,1,1,1,1,6),(-1.,-0.984615384615383,-0.969230769230768,-0.953846153846152,
-0.938461538461537,-0.923076923076922,-0.907692307692306,-0.892307692307691,
-0.876923076923076,-0.86153846153846,-0.846153846153845,-0.83076923076923,
-0.815384615384614,-0.799999999999999,-0.784615384615384,-0.769230769230768,
-0.753846153846153,-0.738461538461538,-0.723076923076922,-0.707692307692307,
-0.692307692307692,-0.676923076923076,-0.661538461538461,-0.646153846153846,
-0.63076923076923,-0.615384615384615,-0.6,-0.584615384615384,-0.569230769230769,
-0.553846153846154,-0.538461538461538,-0.523076923076923,-0.507692307692308,
-0.492307692307692,-0.476923076923077,-0.461538461538462,-0.446153846153846,
-0.430769230769231,-0.415384615384615,-0.4,-0.384615384615385,-0.369230769230769,
-0.353846153846154,-0.338461538461538,-0.323076923076923,-0.307692307692308,
-0.292307692307692,-0.276923076923077,-0.261538461538462,-0.246153846153846,
-0.230769230769231,-0.215384615384615,-0.2,-0.184615384615385,-0.169230769230769,
-0.153846153846154,-0.138461538461538,-0.123076923076923,-0.107692307692308,
-0.0923076923076923,-0.0769230769230769,-0.0615384615384615,-0.0461538461538462,
-0.0307692307692308,-0.0153846153846154,0.),.UNSPECIFIED.)
CURVE()
GEOMETRIC_REPRESENTATION_ITEM()
RATIONAL_B_SPLINE_CURVE((1.,1.,1.,1.,1.,1.,1.,1.,1.,1.,1.,1.,1.,1.,1.,1.,
1.,1.,1.,1.,1.,1.,1.,1.,1.,1.,1.,1.,1.,1.,1.,1.,1.,1.,1.,1.,1.,1.,1.,1.,
1.,1.,1.,1.,1.,1.,1.,1.,1.,1.,1.,1.,1.,1.,1.,1.,1.,1.,1.,1.,1.,1.,1.,1.,
1.,1.,1.,1.,1.,1.))
REPRESENTATION_ITEM('')
);
#121=(
BOUNDED_CURVE()
B_SPLINE_CURVE(5,(#30397,#30398,#30399,#30400,#30401,#30402,#30403,#30404,
#30405,#30406,#30407,#30408,#30409,#30410,#30411,#30412,#30413,#30414,#30415,
#30416,#30417,#30418,#30419,#30420,#30421,#30422,#30423,#30424,#30425,#30426,
#30427,#30428,#30429,#30430,#30431,#30432,#30433,#30434,#30435,#30436,#30437,
#30438,#30439,#30440,#30441,#30442,#30443,#30444,#30445,#30446,#30447,#30448,
#30449,#30450,#30451,#30452,#30453,#30454,#30455,#30456,#30457,#30458,#30459,
#30460,#30461,#30462,#30463,#30464,#30465,#30466),.UNSPECIFIED.,.F.,.F.)
B_SPLINE_CURVE_WITH_KNOTS((6,1,1,1,1,1,1,1,1,1,1,1,1,1,1,1,1,1,1,1,1,1,
1,1,1,1,1,1,1,1,1,1,1,1,1,1,1,1,1,1,1,1,1,1,1,1,1,1,1,1,1,1,1,1,1,1,1,1,
1,1,1,1,1,1,1,6),(-1.,-0.984615384615383,-0.969230769230768,-0.953846153846152,
-0.938461538461537,-0.923076923076922,-0.907692307692306,-0.892307692307691,
-0.876923076923076,-0.86153846153846,-0.846153846153845,-0.83076923076923,
-0.815384615384614,-0.799999999999999,-0.784615384615384,-0.769230769230768,
-0.753846153846153,-0.738461538461538,-0.723076923076922,-0.707692307692307,
-0.692307692307692,-0.676923076923076,-0.661538461538461,-0.646153846153846,
-0.63076923076923,-0.615384615384615,-0.6,-0.584615384615384,-0.569230769230769,
-0.553846153846154,-0.538461538461538,-0.523076923076923,-0.507692307692308,
-0.492307692307692,-0.476923076923077,-0.461538461538462,-0.446153846153846,
-0.430769230769231,-0.415384615384615,-0.4,-0.384615384615385,-0.369230769230769,
-0.353846153846154,-0.338461538461538,-0.323076923076923,-0.307692307692308,
-0.292307692307692,-0.276923076923077,-0.261538461538462,-0.246153846153846,
-0.230769230769231,-0.215384615384615,-0.2,-0.184615384615385,-0.169230769230769,
-0.153846153846154,-0.138461538461538,-0.123076923076923,-0.107692307692308,
-0.0923076923076923,-0.0769230769230769,-0.0615384615384615,-0.0461538461538462,
-0.0307692307692308,-0.0153846153846154,0.),.UNSPECIFIED.)
CURVE()
GEOMETRIC_REPRESENTATION_ITEM()
RATIONAL_B_SPLINE_CURVE((1.,1.,1.,1.,1.,1.,1.,1.,1.,1.,1.,1.,1.,1.,1.,1.,
1.,1.,1.,1.,1.,1.,1.,1.,1.,1.,1.,1.,1.,1.,1.,1.,1.,1.,1.,1.,1.,1.,1.,1.,
1.,1.,1.,1.,1.,1.,1.,1.,1.,1.,1.,1.,1.,1.,1.,1.,1.,1.,1.,1.,1.,1.,1.,1.,
1.,1.,1.,1.,1.,1.))
REPRESENTATION_ITEM('')
);
#122=(
BOUNDED_CURVE()
B_SPLINE_CURVE(5,(#30613,#30614,#30615,#30616,#30617,#30618,#30619,#30620,
#30621,#30622,#30623,#30624,#30625,#30626,#30627,#30628,#30629,#30630,#30631,
#30632,#30633,#30634,#30635,#30636,#30637,#30638,#30639,#30640,#30641,#30642,
#30643,#30644,#30645,#30646,#30647,#30648,#30649,#30650,#30651,#30652,#30653,
#30654,#30655,#30656,#30657,#30658,#30659,#30660,#30661,#30662,#30663,#30664,
#30665,#30666,#30667,#30668,#30669,#30670,#30671,#30672,#30673,#30674,#30675,
#30676,#30677,#30678,#30679,#30680,#30681,#30682),.UNSPECIFIED.,.F.,.F.)
B_SPLINE_CURVE_WITH_KNOTS((6,1,1,1,1,1,1,1,1,1,1,1,1,1,1,1,1,1,1,1,1,1,
1,1,1,1,1,1,1,1,1,1,1,1,1,1,1,1,1,1,1,1,1,1,1,1,1,1,1,1,1,1,1,1,1,1,1,1,
1,1,1,1,1,1,1,6),(-1.,-0.984615384615383,-0.969230769230768,-0.953846153846152,
-0.938461538461537,-0.923076923076922,-0.907692307692306,-0.892307692307691,
-0.876923076923076,-0.86153846153846,-0.846153846153845,-0.83076923076923,
-0.815384615384614,-0.799999999999999,-0.784615384615384,-0.769230769230768,
-0.753846153846153,-0.738461538461538,-0.723076923076922,-0.707692307692307,
-0.692307692307692,-0.676923076923076,-0.661538461538461,-0.646153846153846,
-0.63076923076923,-0.615384615384615,-0.6,-0.584615384615384,-0.569230769230769,
-0.553846153846154,-0.538461538461538,-0.523076923076923,-0.507692307692308,
-0.492307692307692,-0.476923076923077,-0.461538461538462,-0.446153846153846,
-0.430769230769231,-0.415384615384615,-0.4,-0.384615384615385,-0.369230769230769,
-0.353846153846154,-0.338461538461538,-0.323076923076923,-0.307692307692308,
-0.292307692307692,-0.276923076923077,-0.261538461538462,-0.246153846153846,
-0.230769230769231,-0.215384615384615,-0.2,-0.184615384615385,-0.169230769230769,
-0.153846153846154,-0.138461538461538,-0.123076923076923,-0.107692307692308,
-0.0923076923076923,-0.0769230769230769,-0.0615384615384615,-0.0461538461538462,
-0.0307692307692308,-0.0153846153846154,0.),.UNSPECIFIED.)
CURVE()
GEOMETRIC_REPRESENTATION_ITEM()
RATIONAL_B_SPLINE_CURVE((1.,1.,1.,1.,1.,1.,1.,1.,1.,1.,1.,1.,1.,1.,1.,1.,
1.,1.,1.,1.,1.,1.,1.,1.,1.,1.,1.,1.,1.,1.,1.,1.,1.,1.,1.,1.,1.,1.,1.,1.,
1.,1.,1.,1.,1.,1.,1.,1.,1.,1.,1.,1.,1.,1.,1.,1.,1.,1.,1.,1.,1.,1.,1.,1.,
1.,1.,1.,1.,1.,1.))
REPRESENTATION_ITEM('')
);
#123=(
BOUNDED_CURVE()
B_SPLINE_CURVE(5,(#30829,#30830,#30831,#30832,#30833,#30834,#30835,#30836,
#30837,#30838,#30839,#30840,#30841,#30842,#30843,#30844,#30845,#30846,#30847,
#30848,#30849,#30850,#30851,#30852,#30853,#30854,#30855,#30856,#30857,#30858,
#30859,#30860,#30861,#30862,#30863,#30864,#30865,#30866,#30867,#30868,#30869,
#30870,#30871,#30872,#30873,#30874,#30875,#30876,#30877,#30878,#30879,#30880,
#30881,#30882,#30883,#30884,#30885,#30886,#30887,#30888,#30889,#30890,#30891,
#30892,#30893,#30894,#30895,#30896,#30897,#30898),.UNSPECIFIED.,.F.,.F.)
B_SPLINE_CURVE_WITH_KNOTS((6,1,1,1,1,1,1,1,1,1,1,1,1,1,1,1,1,1,1,1,1,1,
1,1,1,1,1,1,1,1,1,1,1,1,1,1,1,1,1,1,1,1,1,1,1,1,1,1,1,1,1,1,1,1,1,1,1,1,
1,1,1,1,1,1,1,6),(-1.,-0.984615384615383,-0.969230769230768,-0.953846153846152,
-0.938461538461537,-0.923076923076922,-0.907692307692306,-0.892307692307691,
-0.876923076923076,-0.86153846153846,-0.846153846153845,-0.83076923076923,
-0.815384615384614,-0.799999999999999,-0.784615384615384,-0.769230769230768,
-0.753846153846153,-0.738461538461538,-0.723076923076922,-0.707692307692307,
-0.692307692307692,-0.676923076923076,-0.661538461538461,-0.646153846153846,
-0.63076923076923,-0.615384615384615,-0.6,-0.584615384615384,-0.569230769230769,
-0.553846153846154,-0.538461538461538,-0.523076923076923,-0.507692307692308,
-0.492307692307692,-0.476923076923077,-0.461538461538462,-0.446153846153846,
-0.430769230769231,-0.415384615384615,-0.4,-0.384615384615385,-0.369230769230769,
-0.353846153846154,-0.338461538461538,-0.323076923076923,-0.307692307692308,
-0.292307692307692,-0.276923076923077,-0.261538461538462,-0.246153846153846,
-0.230769230769231,-0.215384615384615,-0.2,-0.184615384615385,-0.169230769230769,
-0.153846153846154,-0.138461538461538,-0.123076923076923,-0.107692307692308,
-0.0923076923076923,-0.0769230769230769,-0.0615384615384615,-0.0461538461538462,
-0.0307692307692308,-0.0153846153846154,0.),.UNSPECIFIED.)
CURVE()
GEOMETRIC_REPRESENTATION_ITEM()
RATIONAL_B_SPLINE_CURVE((1.,1.,1.,1.,1.,1.,1.,1.,1.,1.,1.,1.,1.,1.,1.,1.,
1.,1.,1.,1.,1.,1.,1.,1.,1.,1.,1.,1.,1.,1.,1.,1.,1.,1.,1.,1.,1.,1.,1.,1.,
1.,1.,1.,1.,1.,1.,1.,1.,1.,1.,1.,1.,1.,1.,1.,1.,1.,1.,1.,1.,1.,1.,1.,1.,
1.,1.,1.,1.,1.,1.))
REPRESENTATION_ITEM('')
);
#124=(
BOUNDED_CURVE()
B_SPLINE_CURVE(5,(#31045,#31046,#31047,#31048,#31049,#31050,#31051,#31052,
#31053,#31054,#31055,#31056,#31057,#31058,#31059,#31060,#31061,#31062,#31063,
#31064,#31065,#31066,#31067,#31068,#31069,#31070,#31071,#31072,#31073,#31074,
#31075,#31076,#31077,#31078,#31079,#31080,#31081,#31082,#31083,#31084,#31085,
#31086,#31087,#31088,#31089,#31090,#31091,#31092,#31093,#31094,#31095,#31096,
#31097,#31098,#31099,#31100,#31101,#31102,#31103,#31104,#31105,#31106,#31107,
#31108,#31109,#31110,#31111,#31112,#31113,#31114),.UNSPECIFIED.,.F.,.F.)
B_SPLINE_CURVE_WITH_KNOTS((6,1,1,1,1,1,1,1,1,1,1,1,1,1,1,1,1,1,1,1,1,1,
1,1,1,1,1,1,1,1,1,1,1,1,1,1,1,1,1,1,1,1,1,1,1,1,1,1,1,1,1,1,1,1,1,1,1,1,
1,1,1,1,1,1,1,6),(-1.,-0.984615384615383,-0.969230769230768,-0.953846153846152,
-0.938461538461537,-0.923076923076922,-0.907692307692306,-0.892307692307691,
-0.876923076923076,-0.86153846153846,-0.846153846153845,-0.83076923076923,
-0.815384615384614,-0.799999999999999,-0.784615384615384,-0.769230769230768,
-0.753846153846153,-0.738461538461538,-0.723076923076922,-0.707692307692307,
-0.692307692307692,-0.676923076923076,-0.661538461538461,-0.646153846153846,
-0.63076923076923,-0.615384615384615,-0.6,-0.584615384615384,-0.569230769230769,
-0.553846153846154,-0.538461538461538,-0.523076923076923,-0.507692307692308,
-0.492307692307692,-0.476923076923077,-0.461538461538462,-0.446153846153846,
-0.430769230769231,-0.415384615384615,-0.4,-0.384615384615385,-0.369230769230769,
-0.353846153846154,-0.338461538461538,-0.323076923076923,-0.307692307692308,
-0.292307692307692,-0.276923076923077,-0.261538461538462,-0.246153846153846,
-0.230769230769231,-0.215384615384615,-0.2,-0.184615384615385,-0.169230769230769,
-0.153846153846154,-0.138461538461538,-0.123076923076923,-0.107692307692308,
-0.0923076923076923,-0.0769230769230769,-0.0615384615384615,-0.0461538461538462,
-0.0307692307692308,-0.0153846153846154,0.),.UNSPECIFIED.)
CURVE()
GEOMETRIC_REPRESENTATION_ITEM()
RATIONAL_B_SPLINE_CURVE((1.,1.,1.,1.,1.,1.,1.,1.,1.,1.,1.,1.,1.,1.,1.,1.,
1.,1.,1.,1.,1.,1.,1.,1.,1.,1.,1.,1.,1.,1.,1.,1.,1.,1.,1.,1.,1.,1.,1.,1.,
1.,1.,1.,1.,1.,1.,1.,1.,1.,1.,1.,1.,1.,1.,1.,1.,1.,1.,1.,1.,1.,1.,1.,1.,
1.,1.,1.,1.,1.,1.))
REPRESENTATION_ITEM('')
);
#125=(
BOUNDED_CURVE()
B_SPLINE_CURVE(5,(#31261,#31262,#31263,#31264,#31265,#31266,#31267,#31268,
#31269,#31270,#31271,#31272,#31273,#31274,#31275,#31276,#31277,#31278,#31279,
#31280,#31281,#31282,#31283,#31284,#31285,#31286,#31287,#31288,#31289,#31290,
#31291,#31292,#31293,#31294,#31295,#31296,#31297,#31298,#31299,#31300,#31301,
#31302,#31303,#31304,#31305,#31306,#31307,#31308,#31309,#31310,#31311,#31312,
#31313,#31314,#31315,#31316,#31317,#31318,#31319,#31320,#31321,#31322,#31323,
#31324,#31325,#31326,#31327,#31328,#31329,#31330),.UNSPECIFIED.,.F.,.F.)
B_SPLINE_CURVE_WITH_KNOTS((6,1,1,1,1,1,1,1,1,1,1,1,1,1,1,1,1,1,1,1,1,1,
1,1,1,1,1,1,1,1,1,1,1,1,1,1,1,1,1,1,1,1,1,1,1,1,1,1,1,1,1,1,1,1,1,1,1,1,
1,1,1,1,1,1,1,6),(-1.,-0.984615384615383,-0.969230769230768,-0.953846153846152,
-0.938461538461537,-0.923076923076922,-0.907692307692306,-0.892307692307691,
-0.876923076923076,-0.86153846153846,-0.846153846153845,-0.83076923076923,
-0.815384615384614,-0.799999999999999,-0.784615384615384,-0.769230769230768,
-0.753846153846153,-0.738461538461538,-0.723076923076922,-0.707692307692307,
-0.692307692307692,-0.676923076923076,-0.661538461538461,-0.646153846153846,
-0.63076923076923,-0.615384615384615,-0.6,-0.584615384615384,-0.569230769230769,
-0.553846153846154,-0.538461538461538,-0.523076923076923,-0.507692307692308,
-0.492307692307692,-0.476923076923077,-0.461538461538462,-0.446153846153846,
-0.430769230769231,-0.415384615384615,-0.4,-0.384615384615385,-0.369230769230769,
-0.353846153846154,-0.338461538461538,-0.323076923076923,-0.307692307692308,
-0.292307692307692,-0.276923076923077,-0.261538461538462,-0.246153846153846,
-0.230769230769231,-0.215384615384615,-0.2,-0.184615384615385,-0.169230769230769,
-0.153846153846154,-0.138461538461538,-0.123076923076923,-0.107692307692308,
-0.0923076923076923,-0.0769230769230769,-0.0615384615384615,-0.0461538461538462,
-0.0307692307692308,-0.0153846153846154,0.),.UNSPECIFIED.)
CURVE()
GEOMETRIC_REPRESENTATION_ITEM()
RATIONAL_B_SPLINE_CURVE((1.,1.,1.,1.,1.,1.,1.,1.,1.,1.,1.,1.,1.,1.,1.,1.,
1.,1.,1.,1.,1.,1.,1.,1.,1.,1.,1.,1.,1.,1.,1.,1.,1.,1.,1.,1.,1.,1.,1.,1.,
1.,1.,1.,1.,1.,1.,1.,1.,1.,1.,1.,1.,1.,1.,1.,1.,1.,1.,1.,1.,1.,1.,1.,1.,
1.,1.,1.,1.,1.,1.))
REPRESENTATION_ITEM('')
);
#126=(
BOUNDED_CURVE()
B_SPLINE_CURVE(5,(#31477,#31478,#31479,#31480,#31481,#31482,#31483,#31484,
#31485,#31486,#31487,#31488,#31489,#31490,#31491,#31492,#31493,#31494,#31495,
#31496,#31497,#31498,#31499,#31500,#31501,#31502,#31503,#31504,#31505,#31506,
#31507,#31508,#31509,#31510,#31511,#31512,#31513,#31514,#31515,#31516,#31517,
#31518,#31519,#31520,#31521,#31522,#31523,#31524,#31525,#31526,#31527,#31528,
#31529,#31530,#31531,#31532,#31533,#31534,#31535,#31536,#31537,#31538,#31539,
#31540,#31541,#31542,#31543,#31544,#31545,#31546),.UNSPECIFIED.,.F.,.F.)
B_SPLINE_CURVE_WITH_KNOTS((6,1,1,1,1,1,1,1,1,1,1,1,1,1,1,1,1,1,1,1,1,1,
1,1,1,1,1,1,1,1,1,1,1,1,1,1,1,1,1,1,1,1,1,1,1,1,1,1,1,1,1,1,1,1,1,1,1,1,
1,1,1,1,1,1,1,6),(-1.,-0.984615384615383,-0.969230769230768,-0.953846153846152,
-0.938461538461537,-0.923076923076922,-0.907692307692306,-0.892307692307691,
-0.876923076923076,-0.86153846153846,-0.846153846153845,-0.83076923076923,
-0.815384615384614,-0.799999999999999,-0.784615384615384,-0.769230769230768,
-0.753846153846153,-0.738461538461538,-0.723076923076922,-0.707692307692307,
-0.692307692307692,-0.676923076923076,-0.661538461538461,-0.646153846153846,
-0.63076923076923,-0.615384615384615,-0.6,-0.584615384615384,-0.569230769230769,
-0.553846153846154,-0.538461538461538,-0.523076923076923,-0.507692307692308,
-0.492307692307692,-0.476923076923077,-0.461538461538462,-0.446153846153846,
-0.430769230769231,-0.415384615384615,-0.4,-0.384615384615385,-0.369230769230769,
-0.353846153846154,-0.338461538461538,-0.323076923076923,-0.307692307692308,
-0.292307692307692,-0.276923076923077,-0.261538461538462,-0.246153846153846,
-0.230769230769231,-0.215384615384615,-0.2,-0.184615384615385,-0.169230769230769,
-0.153846153846154,-0.138461538461538,-0.123076923076923,-0.107692307692308,
-0.0923076923076923,-0.0769230769230769,-0.0615384615384615,-0.0461538461538462,
-0.0307692307692308,-0.0153846153846154,0.),.UNSPECIFIED.)
CURVE()
GEOMETRIC_REPRESENTATION_ITEM()
RATIONAL_B_SPLINE_CURVE((1.,1.,1.,1.,1.,1.,1.,1.,1.,1.,1.,1.,1.,1.,1.,1.,
1.,1.,1.,1.,1.,1.,1.,1.,1.,1.,1.,1.,1.,1.,1.,1.,1.,1.,1.,1.,1.,1.,1.,1.,
1.,1.,1.,1.,1.,1.,1.,1.,1.,1.,1.,1.,1.,1.,1.,1.,1.,1.,1.,1.,1.,1.,1.,1.,
1.,1.,1.,1.,1.,1.))
REPRESENTATION_ITEM('')
);
#127=(
BOUNDED_CURVE()
B_SPLINE_CURVE(5,(#31693,#31694,#31695,#31696,#31697,#31698,#31699,#31700,
#31701,#31702,#31703,#31704,#31705,#31706,#31707,#31708,#31709,#31710,#31711,
#31712,#31713,#31714,#31715,#31716,#31717,#31718,#31719,#31720,#31721,#31722,
#31723,#31724,#31725,#31726,#31727,#31728,#31729,#31730,#31731,#31732,#31733,
#31734,#31735,#31736,#31737,#31738,#31739,#31740,#31741,#31742,#31743,#31744,
#31745,#31746,#31747,#31748,#31749,#31750,#31751,#31752,#31753,#31754,#31755,
#31756,#31757,#31758,#31759,#31760,#31761,#31762),.UNSPECIFIED.,.F.,.F.)
B_SPLINE_CURVE_WITH_KNOTS((6,1,1,1,1,1,1,1,1,1,1,1,1,1,1,1,1,1,1,1,1,1,
1,1,1,1,1,1,1,1,1,1,1,1,1,1,1,1,1,1,1,1,1,1,1,1,1,1,1,1,1,1,1,1,1,1,1,1,
1,1,1,1,1,1,1,6),(-1.,-0.984615384615383,-0.969230769230768,-0.953846153846152,
-0.938461538461537,-0.923076923076922,-0.907692307692306,-0.892307692307691,
-0.876923076923076,-0.86153846153846,-0.846153846153845,-0.83076923076923,
-0.815384615384614,-0.799999999999999,-0.784615384615384,-0.769230769230768,
-0.753846153846153,-0.738461538461538,-0.723076923076922,-0.707692307692307,
-0.692307692307692,-0.676923076923076,-0.661538461538461,-0.646153846153846,
-0.63076923076923,-0.615384615384615,-0.6,-0.584615384615384,-0.569230769230769,
-0.553846153846154,-0.538461538461538,-0.523076923076923,-0.507692307692308,
-0.492307692307692,-0.476923076923077,-0.461538461538462,-0.446153846153846,
-0.430769230769231,-0.415384615384615,-0.4,-0.384615384615385,-0.369230769230769,
-0.353846153846154,-0.338461538461538,-0.323076923076923,-0.307692307692308,
-0.292307692307692,-0.276923076923077,-0.261538461538462,-0.246153846153846,
-0.230769230769231,-0.215384615384615,-0.2,-0.184615384615385,-0.169230769230769,
-0.153846153846154,-0.138461538461538,-0.123076923076923,-0.107692307692308,
-0.0923076923076923,-0.0769230769230769,-0.0615384615384615,-0.0461538461538462,
-0.0307692307692308,-0.0153846153846154,0.),.UNSPECIFIED.)
CURVE()
GEOMETRIC_REPRESENTATION_ITEM()
RATIONAL_B_SPLINE_CURVE((1.,1.,1.,1.,1.,1.,1.,1.,1.,1.,1.,1.,1.,1.,1.,1.,
1.,1.,1.,1.,1.,1.,1.,1.,1.,1.,1.,1.,1.,1.,1.,1.,1.,1.,1.,1.,1.,1.,1.,1.,
1.,1.,1.,1.,1.,1.,1.,1.,1.,1.,1.,1.,1.,1.,1.,1.,1.,1.,1.,1.,1.,1.,1.,1.,
1.,1.,1.,1.,1.,1.))
REPRESENTATION_ITEM('')
);
#128=(
BOUNDED_CURVE()
B_SPLINE_CURVE(5,(#31909,#31910,#31911,#31912,#31913,#31914,#31915,#31916,
#31917,#31918,#31919,#31920,#31921,#31922,#31923,#31924,#31925,#31926,#31927,
#31928,#31929,#31930,#31931,#31932,#31933,#31934,#31935,#31936,#31937,#31938,
#31939,#31940,#31941,#31942,#31943,#31944,#31945,#31946,#31947,#31948,#31949,
#31950,#31951,#31952,#31953,#31954,#31955,#31956,#31957,#31958,#31959,#31960,
#31961,#31962,#31963,#31964,#31965,#31966,#31967,#31968,#31969,#31970,#31971,
#31972,#31973,#31974,#31975,#31976,#31977,#31978),.UNSPECIFIED.,.F.,.F.)
B_SPLINE_CURVE_WITH_KNOTS((6,1,1,1,1,1,1,1,1,1,1,1,1,1,1,1,1,1,1,1,1,1,
1,1,1,1,1,1,1,1,1,1,1,1,1,1,1,1,1,1,1,1,1,1,1,1,1,1,1,1,1,1,1,1,1,1,1,1,
1,1,1,1,1,1,1,6),(-1.,-0.984615384615383,-0.969230769230768,-0.953846153846152,
-0.938461538461537,-0.923076923076922,-0.907692307692306,-0.892307692307691,
-0.876923076923076,-0.86153846153846,-0.846153846153845,-0.83076923076923,
-0.815384615384614,-0.799999999999999,-0.784615384615384,-0.769230769230768,
-0.753846153846153,-0.738461538461538,-0.723076923076922,-0.707692307692307,
-0.692307692307692,-0.676923076923076,-0.661538461538461,-0.646153846153846,
-0.63076923076923,-0.615384615384615,-0.6,-0.584615384615384,-0.569230769230769,
-0.553846153846154,-0.538461538461538,-0.523076923076923,-0.507692307692308,
-0.492307692307692,-0.476923076923077,-0.461538461538462,-0.446153846153846,
-0.430769230769231,-0.415384615384615,-0.4,-0.384615384615385,-0.369230769230769,
-0.353846153846154,-0.338461538461538,-0.323076923076923,-0.307692307692308,
-0.292307692307692,-0.276923076923077,-0.261538461538462,-0.246153846153846,
-0.230769230769231,-0.215384615384615,-0.2,-0.184615384615385,-0.169230769230769,
-0.153846153846154,-0.138461538461538,-0.123076923076923,-0.107692307692308,
-0.0923076923076923,-0.0769230769230769,-0.0615384615384615,-0.0461538461538462,
-0.0307692307692308,-0.0153846153846154,0.),.UNSPECIFIED.)
CURVE()
GEOMETRIC_REPRESENTATION_ITEM()
RATIONAL_B_SPLINE_CURVE((1.,1.,1.,1.,1.,1.,1.,1.,1.,1.,1.,1.,1.,1.,1.,1.,
1.,1.,1.,1.,1.,1.,1.,1.,1.,1.,1.,1.,1.,1.,1.,1.,1.,1.,1.,1.,1.,1.,1.,1.,
1.,1.,1.,1.,1.,1.,1.,1.,1.,1.,1.,1.,1.,1.,1.,1.,1.,1.,1.,1.,1.,1.,1.,1.,
1.,1.,1.,1.,1.,1.))
REPRESENTATION_ITEM('')
);
#129=(
BOUNDED_CURVE()
B_SPLINE_CURVE(5,(#32125,#32126,#32127,#32128,#32129,#32130,#32131,#32132,
#32133,#32134,#32135,#32136,#32137,#32138,#32139,#32140,#32141,#32142,#32143,
#32144,#32145,#32146,#32147,#32148,#32149,#32150,#32151,#32152,#32153,#32154,
#32155,#32156,#32157,#32158,#32159,#32160,#32161,#32162,#32163,#32164,#32165,
#32166,#32167,#32168,#32169,#32170,#32171,#32172,#32173,#32174,#32175,#32176,
#32177,#32178,#32179,#32180,#32181,#32182,#32183,#32184,#32185,#32186,#32187,
#32188,#32189,#32190,#32191,#32192,#32193,#32194),.UNSPECIFIED.,.F.,.F.)
B_SPLINE_CURVE_WITH_KNOTS((6,1,1,1,1,1,1,1,1,1,1,1,1,1,1,1,1,1,1,1,1,1,
1,1,1,1,1,1,1,1,1,1,1,1,1,1,1,1,1,1,1,1,1,1,1,1,1,1,1,1,1,1,1,1,1,1,1,1,
1,1,1,1,1,1,1,6),(-1.,-0.984615384615383,-0.969230769230768,-0.953846153846152,
-0.938461538461537,-0.923076923076922,-0.907692307692306,-0.892307692307691,
-0.876923076923076,-0.86153846153846,-0.846153846153845,-0.83076923076923,
-0.815384615384614,-0.799999999999999,-0.784615384615384,-0.769230769230768,
-0.753846153846153,-0.738461538461538,-0.723076923076922,-0.707692307692307,
-0.692307692307692,-0.676923076923076,-0.661538461538461,-0.646153846153846,
-0.63076923076923,-0.615384615384615,-0.6,-0.584615384615384,-0.569230769230769,
-0.553846153846154,-0.538461538461538,-0.523076923076923,-0.507692307692308,
-0.492307692307692,-0.476923076923077,-0.461538461538462,-0.446153846153846,
-0.430769230769231,-0.415384615384615,-0.4,-0.384615384615385,-0.369230769230769,
-0.353846153846154,-0.338461538461538,-0.323076923076923,-0.307692307692308,
-0.292307692307692,-0.276923076923077,-0.261538461538462,-0.246153846153846,
-0.230769230769231,-0.215384615384615,-0.2,-0.184615384615385,-0.169230769230769,
-0.153846153846154,-0.138461538461538,-0.123076923076923,-0.107692307692308,
-0.0923076923076923,-0.0769230769230769,-0.0615384615384615,-0.0461538461538462,
-0.0307692307692308,-0.0153846153846154,0.),.UNSPECIFIED.)
CURVE()
GEOMETRIC_REPRESENTATION_ITEM()
RATIONAL_B_SPLINE_CURVE((1.,1.,1.,1.,1.,1.,1.,1.,1.,1.,1.,1.,1.,1.,1.,1.,
1.,1.,1.,1.,1.,1.,1.,1.,1.,1.,1.,1.,1.,1.,1.,1.,1.,1.,1.,1.,1.,1.,1.,1.,
1.,1.,1.,1.,1.,1.,1.,1.,1.,1.,1.,1.,1.,1.,1.,1.,1.,1.,1.,1.,1.,1.,1.,1.,
1.,1.,1.,1.,1.,1.))
REPRESENTATION_ITEM('')
);
#130=(
BOUNDED_CURVE()
B_SPLINE_CURVE(5,(#32341,#32342,#32343,#32344,#32345,#32346,#32347,#32348,
#32349,#32350,#32351,#32352,#32353,#32354,#32355,#32356,#32357,#32358,#32359,
#32360,#32361,#32362,#32363,#32364,#32365,#32366,#32367,#32368,#32369,#32370,
#32371,#32372,#32373,#32374,#32375,#32376,#32377,#32378,#32379,#32380,#32381,
#32382,#32383,#32384,#32385,#32386,#32387,#32388,#32389,#32390,#32391,#32392,
#32393,#32394,#32395,#32396,#32397,#32398,#32399,#32400,#32401,#32402,#32403,
#32404,#32405,#32406,#32407,#32408,#32409,#32410),.UNSPECIFIED.,.F.,.F.)
B_SPLINE_CURVE_WITH_KNOTS((6,1,1,1,1,1,1,1,1,1,1,1,1,1,1,1,1,1,1,1,1,1,
1,1,1,1,1,1,1,1,1,1,1,1,1,1,1,1,1,1,1,1,1,1,1,1,1,1,1,1,1,1,1,1,1,1,1,1,
1,1,1,1,1,1,1,6),(-1.,-0.984615384615383,-0.969230769230768,-0.953846153846152,
-0.938461538461537,-0.923076923076922,-0.907692307692306,-0.892307692307691,
-0.876923076923076,-0.86153846153846,-0.846153846153845,-0.83076923076923,
-0.815384615384614,-0.799999999999999,-0.784615384615384,-0.769230769230768,
-0.753846153846153,-0.738461538461538,-0.723076923076922,-0.707692307692307,
-0.692307692307692,-0.676923076923076,-0.661538461538461,-0.646153846153846,
-0.63076923076923,-0.615384615384615,-0.6,-0.584615384615384,-0.569230769230769,
-0.553846153846154,-0.538461538461538,-0.523076923076923,-0.507692307692308,
-0.492307692307692,-0.476923076923077,-0.461538461538462,-0.446153846153846,
-0.430769230769231,-0.415384615384615,-0.4,-0.384615384615385,-0.369230769230769,
-0.353846153846154,-0.338461538461538,-0.323076923076923,-0.307692307692308,
-0.292307692307692,-0.276923076923077,-0.261538461538462,-0.246153846153846,
-0.230769230769231,-0.215384615384615,-0.2,-0.184615384615385,-0.169230769230769,
-0.153846153846154,-0.138461538461538,-0.123076923076923,-0.107692307692308,
-0.0923076923076923,-0.0769230769230769,-0.0615384615384615,-0.0461538461538462,
-0.0307692307692308,-0.0153846153846154,0.),.UNSPECIFIED.)
CURVE()
GEOMETRIC_REPRESENTATION_ITEM()
RATIONAL_B_SPLINE_CURVE((1.,1.,1.,1.,1.,1.,1.,1.,1.,1.,1.,1.,1.,1.,1.,1.,
1.,1.,1.,1.,1.,1.,1.,1.,1.,1.,1.,1.,1.,1.,1.,1.,1.,1.,1.,1.,1.,1.,1.,1.,
1.,1.,1.,1.,1.,1.,1.,1.,1.,1.,1.,1.,1.,1.,1.,1.,1.,1.,1.,1.,1.,1.,1.,1.,
1.,1.,1.,1.,1.,1.))
REPRESENTATION_ITEM('')
);
#131=ITEM_DEFINED_TRANSFORMATION($,$,#13415,#13537);
#132=ITEM_DEFINED_TRANSFORMATION($,$,#13435,#13538);
#133=ITEM_DEFINED_TRANSFORMATION($,$,#13455,#13539);
#134=ITEM_DEFINED_TRANSFORMATION($,$,#13470,#13540);
#135=ITEM_DEFINED_TRANSFORMATION($,$,#13520,#13541);
#136=ITEM_DEFINED_TRANSFORMATION($,$,#13567,#13789);
#137=ITEM_DEFINED_TRANSFORMATION($,$,#13748,#13790);
#138=ITEM_DEFINED_TRANSFORMATION($,$,#13758,#13791);
#139=ITEM_DEFINED_TRANSFORMATION($,$,#13772,#13792);
#140=ITEM_DEFINED_TRANSFORMATION($,$,#13001,#14077);
#141=ITEM_DEFINED_TRANSFORMATION($,$,#13038,#14078);
#142=ITEM_DEFINED_TRANSFORMATION($,$,#13045,#14079);
#143=ITEM_DEFINED_TRANSFORMATION($,$,#13052,#14080);
#144=ITEM_DEFINED_TRANSFORMATION($,$,#13122,#14081);
#145=ITEM_DEFINED_TRANSFORMATION($,$,#13139,#14082);
#146=ITEM_DEFINED_TRANSFORMATION($,$,#13160,#14083);
#147=ITEM_DEFINED_TRANSFORMATION($,$,#13177,#14084);
#148=ITEM_DEFINED_TRANSFORMATION($,$,#13198,#14085);
#149=ITEM_DEFINED_TRANSFORMATION($,$,#13218,#14086);
#150=ITEM_DEFINED_TRANSFORMATION($,$,#13253,#14087);
#151=ITEM_DEFINED_TRANSFORMATION($,$,#13278,#14088);
#152=ITEM_DEFINED_TRANSFORMATION($,$,#13303,#14089);
#153=ITEM_DEFINED_TRANSFORMATION($,$,#13338,#14090);
#154=ITEM_DEFINED_TRANSFORMATION($,$,#13363,#14091);
#155=ITEM_DEFINED_TRANSFORMATION($,$,#13388,#14092);
#156=ITEM_DEFINED_TRANSFORMATION($,$,#13388,#14093);
#157=ITEM_DEFINED_TRANSFORMATION($,$,#13388,#14094);
#158=ITEM_DEFINED_TRANSFORMATION($,$,#13388,#14095);
#159=ITEM_DEFINED_TRANSFORMATION($,$,#13542,#14096);
#160=ITEM_DEFINED_TRANSFORMATION($,$,#13542,#14097);
#161=ITEM_DEFINED_TRANSFORMATION($,$,#13542,#14098);
#162=ITEM_DEFINED_TRANSFORMATION($,$,#13542,#14099);
#163=ITEM_DEFINED_TRANSFORMATION($,$,#13542,#14100);
#164=ITEM_DEFINED_TRANSFORMATION($,$,#13542,#14101);
#165=ITEM_DEFINED_TRANSFORMATION($,$,#14051,#14102);
#166=ITEM_DEFINED_TRANSFORMATION($,$,#14051,#14103);
#167=ITEM_DEFINED_TRANSFORMATION($,$,#13414,#14104);
#168=ITEM_DEFINED_TRANSFORMATION($,$,#13542,#14105);
#169=ITEM_DEFINED_TRANSFORMATION($,$,#13542,#14106);
#170=ITEM_DEFINED_TRANSFORMATION($,$,#13542,#14107);
#171=ITEM_DEFINED_TRANSFORMATION($,$,#13542,#14108);
#172=ITEM_DEFINED_TRANSFORMATION($,$,#13542,#14109);
#173=ITEM_DEFINED_TRANSFORMATION($,$,#13542,#14110);
#174=ITEM_DEFINED_TRANSFORMATION($,$,#13542,#14111);
#175=ITEM_DEFINED_TRANSFORMATION($,$,#13542,#14112);
#176=ITEM_DEFINED_TRANSFORMATION($,$,#14051,#14113);
#177=ITEM_DEFINED_TRANSFORMATION($,$,#14051,#14114);
#178=ITEM_DEFINED_TRANSFORMATION($,$,#13414,#14115);
#179=ITEM_DEFINED_TRANSFORMATION($,$,#13542,#14116);
#180=ITEM_DEFINED_TRANSFORMATION($,$,#13542,#14117);
#181=ITEM_DEFINED_TRANSFORMATION($,$,#13542,#14118);
#182=ITEM_DEFINED_TRANSFORMATION($,$,#13542,#14119);
#183=ITEM_DEFINED_TRANSFORMATION($,$,#13542,#14120);
#184=ITEM_DEFINED_TRANSFORMATION($,$,#13542,#14121);
#185=ITEM_DEFINED_TRANSFORMATION($,$,#13542,#14122);
#186=ITEM_DEFINED_TRANSFORMATION($,$,#13542,#14123);
#187=ITEM_DEFINED_TRANSFORMATION($,$,#13794,#14124);
#188=ITEM_DEFINED_TRANSFORMATION($,$,#13822,#14125);
#189=ITEM_DEFINED_TRANSFORMATION($,$,#13831,#14126);
#190=ITEM_DEFINED_TRANSFORMATION($,$,#13840,#14127);
#191=ITEM_DEFINED_TRANSFORMATION($,$,#13849,#14128);
#192=ITEM_DEFINED_TRANSFORMATION($,$,#13858,#14129);
#193=ITEM_DEFINED_TRANSFORMATION($,$,#13865,#14130);
#194=ITEM_DEFINED_TRANSFORMATION($,$,#13872,#14131);
#195=ITEM_DEFINED_TRANSFORMATION($,$,#13896,#14132);
#196=ITEM_DEFINED_TRANSFORMATION($,$,#13905,#14133);
#197=ITEM_DEFINED_TRANSFORMATION($,$,#13914,#14134);
#198=ITEM_DEFINED_TRANSFORMATION($,$,#13923,#14135);
#199=ITEM_DEFINED_TRANSFORMATION($,$,#14016,#14136);
#200=ITEM_DEFINED_TRANSFORMATION($,$,#14025,#14137);
#201=ITEM_DEFINED_TRANSFORMATION($,$,#14051,#14138);
#202=ITEM_DEFINED_TRANSFORMATION($,$,#14051,#14139);
#203=ITEM_DEFINED_TRANSFORMATION($,$,#14141,#14150);
#204=ITEM_DEFINED_TRANSFORMATION($,$,#13000,#14151);
#205=ITEM_DEFINED_TRANSFORMATION($,$,#13566,#14152);
#206=ITEM_DEFINED_TRANSFORMATION($,$,#13793,#14153);
#207=ITEM_DEFINED_TRANSFORMATION($,$,#14140,#14154);
#208=(
REPRESENTATION_RELATIONSHIP($,$,#32948,#32947)
REPRESENTATION_RELATIONSHIP_WITH_TRANSFORMATION(#131)
SHAPE_REPRESENTATION_RELATIONSHIP()
);
#209=(
REPRESENTATION_RELATIONSHIP($,$,#32949,#32947)
REPRESENTATION_RELATIONSHIP_WITH_TRANSFORMATION(#132)
SHAPE_REPRESENTATION_RELATIONSHIP()
);
#210=(
REPRESENTATION_RELATIONSHIP($,$,#32950,#32947)
REPRESENTATION_RELATIONSHIP_WITH_TRANSFORMATION(#133)
SHAPE_REPRESENTATION_RELATIONSHIP()
);
#211=(
REPRESENTATION_RELATIONSHIP($,$,#32951,#32947)
REPRESENTATION_RELATIONSHIP_WITH_TRANSFORMATION(#134)
SHAPE_REPRESENTATION_RELATIONSHIP()
);
#212=(
REPRESENTATION_RELATIONSHIP($,$,#32952,#32947)
REPRESENTATION_RELATIONSHIP_WITH_TRANSFORMATION(#135)
SHAPE_REPRESENTATION_RELATIONSHIP()
);
#213=(
REPRESENTATION_RELATIONSHIP($,$,#32955,#32954)
REPRESENTATION_RELATIONSHIP_WITH_TRANSFORMATION(#136)
SHAPE_REPRESENTATION_RELATIONSHIP()
);
#214=(
REPRESENTATION_RELATIONSHIP($,$,#32956,#32954)
REPRESENTATION_RELATIONSHIP_WITH_TRANSFORMATION(#137)
SHAPE_REPRESENTATION_RELATIONSHIP()
);
#215=(
REPRESENTATION_RELATIONSHIP($,$,#32957,#32954)
REPRESENTATION_RELATIONSHIP_WITH_TRANSFORMATION(#138)
SHAPE_REPRESENTATION_RELATIONSHIP()
);
#216=(
REPRESENTATION_RELATIONSHIP($,$,#32958,#32954)
REPRESENTATION_RELATIONSHIP_WITH_TRANSFORMATION(#139)
SHAPE_REPRESENTATION_RELATIONSHIP()
);
#217=(
REPRESENTATION_RELATIONSHIP($,$,#32931,#32930)
REPRESENTATION_RELATIONSHIP_WITH_TRANSFORMATION(#140)
SHAPE_REPRESENTATION_RELATIONSHIP()
);
#218=(
REPRESENTATION_RELATIONSHIP($,$,#32932,#32930)
REPRESENTATION_RELATIONSHIP_WITH_TRANSFORMATION(#141)
SHAPE_REPRESENTATION_RELATIONSHIP()
);
#219=(
REPRESENTATION_RELATIONSHIP($,$,#32933,#32930)
REPRESENTATION_RELATIONSHIP_WITH_TRANSFORMATION(#142)
SHAPE_REPRESENTATION_RELATIONSHIP()
);
#220=(
REPRESENTATION_RELATIONSHIP($,$,#32934,#32930)
REPRESENTATION_RELATIONSHIP_WITH_TRANSFORMATION(#143)
SHAPE_REPRESENTATION_RELATIONSHIP()
);
#221=(
REPRESENTATION_RELATIONSHIP($,$,#32935,#32930)
REPRESENTATION_RELATIONSHIP_WITH_TRANSFORMATION(#144)
SHAPE_REPRESENTATION_RELATIONSHIP()
);
#222=(
REPRESENTATION_RELATIONSHIP($,$,#32936,#32930)
REPRESENTATION_RELATIONSHIP_WITH_TRANSFORMATION(#145)
SHAPE_REPRESENTATION_RELATIONSHIP()
);
#223=(
REPRESENTATION_RELATIONSHIP($,$,#32937,#32930)
REPRESENTATION_RELATIONSHIP_WITH_TRANSFORMATION(#146)
SHAPE_REPRESENTATION_RELATIONSHIP()
);
#224=(
REPRESENTATION_RELATIONSHIP($,$,#32938,#32930)
REPRESENTATION_RELATIONSHIP_WITH_TRANSFORMATION(#147)
SHAPE_REPRESENTATION_RELATIONSHIP()
);
#225=(
REPRESENTATION_RELATIONSHIP($,$,#32939,#32930)
REPRESENTATION_RELATIONSHIP_WITH_TRANSFORMATION(#148)
SHAPE_REPRESENTATION_RELATIONSHIP()
);
#226=(
REPRESENTATION_RELATIONSHIP($,$,#32940,#32930)
REPRESENTATION_RELATIONSHIP_WITH_TRANSFORMATION(#149)
SHAPE_REPRESENTATION_RELATIONSHIP()
);
#227=(
REPRESENTATION_RELATIONSHIP($,$,#32941,#32930)
REPRESENTATION_RELATIONSHIP_WITH_TRANSFORMATION(#150)
SHAPE_REPRESENTATION_RELATIONSHIP()
);
#228=(
REPRESENTATION_RELATIONSHIP($,$,#32942,#32930)
REPRESENTATION_RELATIONSHIP_WITH_TRANSFORMATION(#151)
SHAPE_REPRESENTATION_RELATIONSHIP()
);
#229=(
REPRESENTATION_RELATIONSHIP($,$,#32943,#32930)
REPRESENTATION_RELATIONSHIP_WITH_TRANSFORMATION(#152)
SHAPE_REPRESENTATION_RELATIONSHIP()
);
#230=(
REPRESENTATION_RELATIONSHIP($,$,#32944,#32930)
REPRESENTATION_RELATIONSHIP_WITH_TRANSFORMATION(#153)
SHAPE_REPRESENTATION_RELATIONSHIP()
);
#231=(
REPRESENTATION_RELATIONSHIP($,$,#32945,#32930)
REPRESENTATION_RELATIONSHIP_WITH_TRANSFORMATION(#154)
SHAPE_REPRESENTATION_RELATIONSHIP()
);
#232=(
REPRESENTATION_RELATIONSHIP($,$,#32946,#32930)
REPRESENTATION_RELATIONSHIP_WITH_TRANSFORMATION(#155)
SHAPE_REPRESENTATION_RELATIONSHIP()
);
#233=(
REPRESENTATION_RELATIONSHIP($,$,#32946,#32930)
REPRESENTATION_RELATIONSHIP_WITH_TRANSFORMATION(#156)
SHAPE_REPRESENTATION_RELATIONSHIP()
);
#234=(
REPRESENTATION_RELATIONSHIP($,$,#32946,#32930)
REPRESENTATION_RELATIONSHIP_WITH_TRANSFORMATION(#157)
SHAPE_REPRESENTATION_RELATIONSHIP()
);
#235=(
REPRESENTATION_RELATIONSHIP($,$,#32946,#32930)
REPRESENTATION_RELATIONSHIP_WITH_TRANSFORMATION(#158)
SHAPE_REPRESENTATION_RELATIONSHIP()
);
#236=(
REPRESENTATION_RELATIONSHIP($,$,#32953,#32930)
REPRESENTATION_RELATIONSHIP_WITH_TRANSFORMATION(#159)
SHAPE_REPRESENTATION_RELATIONSHIP()
);
#237=(
REPRESENTATION_RELATIONSHIP($,$,#32953,#32930)
REPRESENTATION_RELATIONSHIP_WITH_TRANSFORMATION(#160)
SHAPE_REPRESENTATION_RELATIONSHIP()
);
#238=(
REPRESENTATION_RELATIONSHIP($,$,#32953,#32930)
REPRESENTATION_RELATIONSHIP_WITH_TRANSFORMATION(#161)
SHAPE_REPRESENTATION_RELATIONSHIP()
);
#239=(
REPRESENTATION_RELATIONSHIP($,$,#32953,#32930)
REPRESENTATION_RELATIONSHIP_WITH_TRANSFORMATION(#162)
SHAPE_REPRESENTATION_RELATIONSHIP()
);
#240=(
REPRESENTATION_RELATIONSHIP($,$,#32953,#32930)
REPRESENTATION_RELATIONSHIP_WITH_TRANSFORMATION(#163)
SHAPE_REPRESENTATION_RELATIONSHIP()
);
#241=(
REPRESENTATION_RELATIONSHIP($,$,#32953,#32930)
REPRESENTATION_RELATIONSHIP_WITH_TRANSFORMATION(#164)
SHAPE_REPRESENTATION_RELATIONSHIP()
);
#242=(
REPRESENTATION_RELATIONSHIP($,$,#32974,#32930)
REPRESENTATION_RELATIONSHIP_WITH_TRANSFORMATION(#165)
SHAPE_REPRESENTATION_RELATIONSHIP()
);
#243=(
REPRESENTATION_RELATIONSHIP($,$,#32974,#32930)
REPRESENTATION_RELATIONSHIP_WITH_TRANSFORMATION(#166)
SHAPE_REPRESENTATION_RELATIONSHIP()
);
#244=(
REPRESENTATION_RELATIONSHIP($,$,#32947,#32930)
REPRESENTATION_RELATIONSHIP_WITH_TRANSFORMATION(#167)
SHAPE_REPRESENTATION_RELATIONSHIP()
);
#245=(
REPRESENTATION_RELATIONSHIP($,$,#32953,#32930)
REPRESENTATION_RELATIONSHIP_WITH_TRANSFORMATION(#168)
SHAPE_REPRESENTATION_RELATIONSHIP()
);
#246=(
REPRESENTATION_RELATIONSHIP($,$,#32953,#32930)
REPRESENTATION_RELATIONSHIP_WITH_TRANSFORMATION(#169)
SHAPE_REPRESENTATION_RELATIONSHIP()
);
#247=(
REPRESENTATION_RELATIONSHIP($,$,#32953,#32930)
REPRESENTATION_RELATIONSHIP_WITH_TRANSFORMATION(#170)
SHAPE_REPRESENTATION_RELATIONSHIP()
);
#248=(
REPRESENTATION_RELATIONSHIP($,$,#32953,#32930)
REPRESENTATION_RELATIONSHIP_WITH_TRANSFORMATION(#171)
SHAPE_REPRESENTATION_RELATIONSHIP()
);
#249=(
REPRESENTATION_RELATIONSHIP($,$,#32953,#32930)
REPRESENTATION_RELATIONSHIP_WITH_TRANSFORMATION(#172)
SHAPE_REPRESENTATION_RELATIONSHIP()
);
#250=(
REPRESENTATION_RELATIONSHIP($,$,#32953,#32930)
REPRESENTATION_RELATIONSHIP_WITH_TRANSFORMATION(#173)
SHAPE_REPRESENTATION_RELATIONSHIP()
);
#251=(
REPRESENTATION_RELATIONSHIP($,$,#32953,#32930)
REPRESENTATION_RELATIONSHIP_WITH_TRANSFORMATION(#174)
SHAPE_REPRESENTATION_RELATIONSHIP()
);
#252=(
REPRESENTATION_RELATIONSHIP($,$,#32953,#32930)
REPRESENTATION_RELATIONSHIP_WITH_TRANSFORMATION(#175)
SHAPE_REPRESENTATION_RELATIONSHIP()
);
#253=(
REPRESENTATION_RELATIONSHIP($,$,#32974,#32930)
REPRESENTATION_RELATIONSHIP_WITH_TRANSFORMATION(#176)
SHAPE_REPRESENTATION_RELATIONSHIP()
);
#254=(
REPRESENTATION_RELATIONSHIP($,$,#32974,#32930)
REPRESENTATION_RELATIONSHIP_WITH_TRANSFORMATION(#177)
SHAPE_REPRESENTATION_RELATIONSHIP()
);
#255=(
REPRESENTATION_RELATIONSHIP($,$,#32947,#32930)
REPRESENTATION_RELATIONSHIP_WITH_TRANSFORMATION(#178)
SHAPE_REPRESENTATION_RELATIONSHIP()
);
#256=(
REPRESENTATION_RELATIONSHIP($,$,#32953,#32930)
REPRESENTATION_RELATIONSHIP_WITH_TRANSFORMATION(#179)
SHAPE_REPRESENTATION_RELATIONSHIP()
);
#257=(
REPRESENTATION_RELATIONSHIP($,$,#32953,#32930)
REPRESENTATION_RELATIONSHIP_WITH_TRANSFORMATION(#180)
SHAPE_REPRESENTATION_RELATIONSHIP()
);
#258=(
REPRESENTATION_RELATIONSHIP($,$,#32953,#32930)
REPRESENTATION_RELATIONSHIP_WITH_TRANSFORMATION(#181)
SHAPE_REPRESENTATION_RELATIONSHIP()
);
#259=(
REPRESENTATION_RELATIONSHIP($,$,#32953,#32930)
REPRESENTATION_RELATIONSHIP_WITH_TRANSFORMATION(#182)
SHAPE_REPRESENTATION_RELATIONSHIP()
);
#260=(
REPRESENTATION_RELATIONSHIP($,$,#32953,#32930)
REPRESENTATION_RELATIONSHIP_WITH_TRANSFORMATION(#183)
SHAPE_REPRESENTATION_RELATIONSHIP()
);
#261=(
REPRESENTATION_RELATIONSHIP($,$,#32953,#32930)
REPRESENTATION_RELATIONSHIP_WITH_TRANSFORMATION(#184)
SHAPE_REPRESENTATION_RELATIONSHIP()
);
#262=(
REPRESENTATION_RELATIONSHIP($,$,#32953,#32930)
REPRESENTATION_RELATIONSHIP_WITH_TRANSFORMATION(#185)
SHAPE_REPRESENTATION_RELATIONSHIP()
);
#263=(
REPRESENTATION_RELATIONSHIP($,$,#32953,#32930)
REPRESENTATION_RELATIONSHIP_WITH_TRANSFORMATION(#186)
SHAPE_REPRESENTATION_RELATIONSHIP()
);
#264=(
REPRESENTATION_RELATIONSHIP($,$,#32960,#32959)
REPRESENTATION_RELATIONSHIP_WITH_TRANSFORMATION(#187)
SHAPE_REPRESENTATION_RELATIONSHIP()
);
#265=(
REPRESENTATION_RELATIONSHIP($,$,#32961,#32959)
REPRESENTATION_RELATIONSHIP_WITH_TRANSFORMATION(#188)
SHAPE_REPRESENTATION_RELATIONSHIP()
);
#266=(
REPRESENTATION_RELATIONSHIP($,$,#32962,#32959)
REPRESENTATION_RELATIONSHIP_WITH_TRANSFORMATION(#189)
SHAPE_REPRESENTATION_RELATIONSHIP()
);
#267=(
REPRESENTATION_RELATIONSHIP($,$,#32963,#32959)
REPRESENTATION_RELATIONSHIP_WITH_TRANSFORMATION(#190)
SHAPE_REPRESENTATION_RELATIONSHIP()
);
#268=(
REPRESENTATION_RELATIONSHIP($,$,#32964,#32959)
REPRESENTATION_RELATIONSHIP_WITH_TRANSFORMATION(#191)
SHAPE_REPRESENTATION_RELATIONSHIP()
);
#269=(
REPRESENTATION_RELATIONSHIP($,$,#32965,#32959)
REPRESENTATION_RELATIONSHIP_WITH_TRANSFORMATION(#192)
SHAPE_REPRESENTATION_RELATIONSHIP()
);
#270=(
REPRESENTATION_RELATIONSHIP($,$,#32966,#32959)
REPRESENTATION_RELATIONSHIP_WITH_TRANSFORMATION(#193)
SHAPE_REPRESENTATION_RELATIONSHIP()
);
#271=(
REPRESENTATION_RELATIONSHIP($,$,#32967,#32959)
REPRESENTATION_RELATIONSHIP_WITH_TRANSFORMATION(#194)
SHAPE_REPRESENTATION_RELATIONSHIP()
);
#272=(
REPRESENTATION_RELATIONSHIP($,$,#32968,#32959)
REPRESENTATION_RELATIONSHIP_WITH_TRANSFORMATION(#195)
SHAPE_REPRESENTATION_RELATIONSHIP()
);
#273=(
REPRESENTATION_RELATIONSHIP($,$,#32969,#32959)
REPRESENTATION_RELATIONSHIP_WITH_TRANSFORMATION(#196)
SHAPE_REPRESENTATION_RELATIONSHIP()
);
#274=(
REPRESENTATION_RELATIONSHIP($,$,#32970,#32959)
REPRESENTATION_RELATIONSHIP_WITH_TRANSFORMATION(#197)
SHAPE_REPRESENTATION_RELATIONSHIP()
);
#275=(
REPRESENTATION_RELATIONSHIP($,$,#32971,#32959)
REPRESENTATION_RELATIONSHIP_WITH_TRANSFORMATION(#198)
SHAPE_REPRESENTATION_RELATIONSHIP()
);
#276=(
REPRESENTATION_RELATIONSHIP($,$,#32972,#32959)
REPRESENTATION_RELATIONSHIP_WITH_TRANSFORMATION(#199)
SHAPE_REPRESENTATION_RELATIONSHIP()
);
#277=(
REPRESENTATION_RELATIONSHIP($,$,#32973,#32959)
REPRESENTATION_RELATIONSHIP_WITH_TRANSFORMATION(#200)
SHAPE_REPRESENTATION_RELATIONSHIP()
);
#278=(
REPRESENTATION_RELATIONSHIP($,$,#32974,#32959)
REPRESENTATION_RELATIONSHIP_WITH_TRANSFORMATION(#201)
SHAPE_REPRESENTATION_RELATIONSHIP()
);
#279=(
REPRESENTATION_RELATIONSHIP($,$,#32974,#32959)
REPRESENTATION_RELATIONSHIP_WITH_TRANSFORMATION(#202)
SHAPE_REPRESENTATION_RELATIONSHIP()
);
#280=(
REPRESENTATION_RELATIONSHIP($,$,#32976,#32975)
REPRESENTATION_RELATIONSHIP_WITH_TRANSFORMATION(#203)
SHAPE_REPRESENTATION_RELATIONSHIP()
);
#281=(
REPRESENTATION_RELATIONSHIP($,$,#32930,#32929)
REPRESENTATION_RELATIONSHIP_WITH_TRANSFORMATION(#204)
SHAPE_REPRESENTATION_RELATIONSHIP()
);
#282=(
REPRESENTATION_RELATIONSHIP($,$,#32954,#32929)
REPRESENTATION_RELATIONSHIP_WITH_TRANSFORMATION(#205)
SHAPE_REPRESENTATION_RELATIONSHIP()
);
#283=(
REPRESENTATION_RELATIONSHIP($,$,#32959,#32929)
REPRESENTATION_RELATIONSHIP_WITH_TRANSFORMATION(#206)
SHAPE_REPRESENTATION_RELATIONSHIP()
);
#284=(
REPRESENTATION_RELATIONSHIP($,$,#32975,#32929)
REPRESENTATION_RELATIONSHIP_WITH_TRANSFORMATION(#207)
SHAPE_REPRESENTATION_RELATIONSHIP()
);
#285=CONTEXT_DEPENDENT_SHAPE_REPRESENTATION(#208,#32828);
#286=CONTEXT_DEPENDENT_SHAPE_REPRESENTATION(#209,#32829);
#287=CONTEXT_DEPENDENT_SHAPE_REPRESENTATION(#210,#32830);
#288=CONTEXT_DEPENDENT_SHAPE_REPRESENTATION(#211,#32831);
#289=CONTEXT_DEPENDENT_SHAPE_REPRESENTATION(#212,#32832);
#290=CONTEXT_DEPENDENT_SHAPE_REPRESENTATION(#213,#32839);
#291=CONTEXT_DEPENDENT_SHAPE_REPRESENTATION(#214,#32840);
#292=CONTEXT_DEPENDENT_SHAPE_REPRESENTATION(#215,#32841);
#293=CONTEXT_DEPENDENT_SHAPE_REPRESENTATION(#216,#32842);
#294=CONTEXT_DEPENDENT_SHAPE_REPRESENTATION(#217,#32859);
#295=CONTEXT_DEPENDENT_SHAPE_REPRESENTATION(#218,#32860);
#296=CONTEXT_DEPENDENT_SHAPE_REPRESENTATION(#219,#32861);
#297=CONTEXT_DEPENDENT_SHAPE_REPRESENTATION(#220,#32862);
#298=CONTEXT_DEPENDENT_SHAPE_REPRESENTATION(#221,#32863);
#299=CONTEXT_DEPENDENT_SHAPE_REPRESENTATION(#222,#32864);
#300=CONTEXT_DEPENDENT_SHAPE_REPRESENTATION(#223,#32865);
#301=CONTEXT_DEPENDENT_SHAPE_REPRESENTATION(#224,#32866);
#302=CONTEXT_DEPENDENT_SHAPE_REPRESENTATION(#225,#32867);
#303=CONTEXT_DEPENDENT_SHAPE_REPRESENTATION(#226,#32868);
#304=CONTEXT_DEPENDENT_SHAPE_REPRESENTATION(#227,#32869);
#305=CONTEXT_DEPENDENT_SHAPE_REPRESENTATION(#228,#32870);
#306=CONTEXT_DEPENDENT_SHAPE_REPRESENTATION(#229,#32871);
#307=CONTEXT_DEPENDENT_SHAPE_REPRESENTATION(#230,#32872);
#308=CONTEXT_DEPENDENT_SHAPE_REPRESENTATION(#231,#32873);
#309=CONTEXT_DEPENDENT_SHAPE_REPRESENTATION(#232,#32874);
#310=CONTEXT_DEPENDENT_SHAPE_REPRESENTATION(#233,#32875);
#311=CONTEXT_DEPENDENT_SHAPE_REPRESENTATION(#234,#32876);
#312=CONTEXT_DEPENDENT_SHAPE_REPRESENTATION(#235,#32877);
#313=CONTEXT_DEPENDENT_SHAPE_REPRESENTATION(#236,#32878);
#314=CONTEXT_DEPENDENT_SHAPE_REPRESENTATION(#237,#32879);
#315=CONTEXT_DEPENDENT_SHAPE_REPRESENTATION(#238,#32880);
#316=CONTEXT_DEPENDENT_SHAPE_REPRESENTATION(#239,#32881);
#317=CONTEXT_DEPENDENT_SHAPE_REPRESENTATION(#240,#32882);
#318=CONTEXT_DEPENDENT_SHAPE_REPRESENTATION(#241,#32883);
#319=CONTEXT_DEPENDENT_SHAPE_REPRESENTATION(#242,#32884);
#320=CONTEXT_DEPENDENT_SHAPE_REPRESENTATION(#243,#32885);
#321=CONTEXT_DEPENDENT_SHAPE_REPRESENTATION(#244,#32886);
#322=CONTEXT_DEPENDENT_SHAPE_REPRESENTATION(#245,#32887);
#323=CONTEXT_DEPENDENT_SHAPE_REPRESENTATION(#246,#32888);
#324=CONTEXT_DEPENDENT_SHAPE_REPRESENTATION(#247,#32889);
#325=CONTEXT_DEPENDENT_SHAPE_REPRESENTATION(#248,#32890);
#326=CONTEXT_DEPENDENT_SHAPE_REPRESENTATION(#249,#32891);
#327=CONTEXT_DEPENDENT_SHAPE_REPRESENTATION(#250,#32892);
#328=CONTEXT_DEPENDENT_SHAPE_REPRESENTATION(#251,#32893);
#329=CONTEXT_DEPENDENT_SHAPE_REPRESENTATION(#252,#32894);
#330=CONTEXT_DEPENDENT_SHAPE_REPRESENTATION(#253,#32895);
#331=CONTEXT_DEPENDENT_SHAPE_REPRESENTATION(#254,#32896);
#332=CONTEXT_DEPENDENT_SHAPE_REPRESENTATION(#255,#32897);
#333=CONTEXT_DEPENDENT_SHAPE_REPRESENTATION(#256,#32898);
#334=CONTEXT_DEPENDENT_SHAPE_REPRESENTATION(#257,#32899);
#335=CONTEXT_DEPENDENT_SHAPE_REPRESENTATION(#258,#32900);
#336=CONTEXT_DEPENDENT_SHAPE_REPRESENTATION(#259,#32901);
#337=CONTEXT_DEPENDENT_SHAPE_REPRESENTATION(#260,#32902);
#338=CONTEXT_DEPENDENT_SHAPE_REPRESENTATION(#261,#32903);
#339=CONTEXT_DEPENDENT_SHAPE_REPRESENTATION(#262,#32904);
#340=CONTEXT_DEPENDENT_SHAPE_REPRESENTATION(#263,#32905);
#341=CONTEXT_DEPENDENT_SHAPE_REPRESENTATION(#264,#32906);
#342=CONTEXT_DEPENDENT_SHAPE_REPRESENTATION(#265,#32907);
#343=CONTEXT_DEPENDENT_SHAPE_REPRESENTATION(#266,#32908);
#344=CONTEXT_DEPENDENT_SHAPE_REPRESENTATION(#267,#32909);
#345=CONTEXT_DEPENDENT_SHAPE_REPRESENTATION(#268,#32910);
#346=CONTEXT_DEPENDENT_SHAPE_REPRESENTATION(#269,#32911);
#347=CONTEXT_DEPENDENT_SHAPE_REPRESENTATION(#270,#32912);
#348=CONTEXT_DEPENDENT_SHAPE_REPRESENTATION(#271,#32913);
#349=CONTEXT_DEPENDENT_SHAPE_REPRESENTATION(#272,#32914);
#350=CONTEXT_DEPENDENT_SHAPE_REPRESENTATION(#273,#32915);
#351=CONTEXT_DEPENDENT_SHAPE_REPRESENTATION(#274,#32916);
#352=CONTEXT_DEPENDENT_SHAPE_REPRESENTATION(#275,#32917);
#353=CONTEXT_DEPENDENT_SHAPE_REPRESENTATION(#276,#32918);
#354=CONTEXT_DEPENDENT_SHAPE_REPRESENTATION(#277,#32919);
#355=CONTEXT_DEPENDENT_SHAPE_REPRESENTATION(#278,#32920);
#356=CONTEXT_DEPENDENT_SHAPE_REPRESENTATION(#279,#32921);
#357=CONTEXT_DEPENDENT_SHAPE_REPRESENTATION(#280,#32924);
#358=CONTEXT_DEPENDENT_SHAPE_REPRESENTATION(#281,#32925);
#359=CONTEXT_DEPENDENT_SHAPE_REPRESENTATION(#282,#32926);
#360=CONTEXT_DEPENDENT_SHAPE_REPRESENTATION(#283,#32927);
#361=CONTEXT_DEPENDENT_SHAPE_REPRESENTATION(#284,#32928);
#362=NEXT_ASSEMBLY_USAGE_OCCURRENCE('Inner ring:1','Inner ring:1',
'Inner ring:1',#32996,#32997,'Inner ring:1');
#363=NEXT_ASSEMBLY_USAGE_OCCURRENCE('Outer ring:1','Outer ring:1',
'Outer ring:1',#32996,#32998,'Outer ring:1');
#364=NEXT_ASSEMBLY_USAGE_OCCURRENCE('Balls:1','Balls:1','Balls:1',#32996,
#32999,'Balls:1');
#365=NEXT_ASSEMBLY_USAGE_OCCURRENCE('Cage:1','Cage:1','Cage:1',#32996,#33000,
'Cage:1');
#366=NEXT_ASSEMBLY_USAGE_OCCURRENCE('Seals 2RS:1','Seals 2RS:1',
'Seals 2RS:1',#32996,#33001,'Seals 2RS:1');
#367=NEXT_ASSEMBLY_USAGE_OCCURRENCE('Rack ram:1','Rack ram:1',
'Rack ram:1',#33003,#33004,'Rack ram:1');
#368=NEXT_ASSEMBLY_USAGE_OCCURRENCE('Pressure foot:1','Pressure foot:1',
'Pressure foot:1',#33003,#33005,'Pressure foot:1');
#369=NEXT_ASSEMBLY_USAGE_OCCURRENCE('Upper travel collar:1',
'Upper travel collar:1','Upper travel collar:1',#33003,#33006,
'Upper travel collar:1');
#370=NEXT_ASSEMBLY_USAGE_OCCURRENCE('Socket Set Screw - M4x6:2',
'Socket Set Screw - M4x6:2','Socket Set Screw - M4x6:2',#33003,#33007,
'Socket Set Screw - M4x6:2');
#371=NEXT_ASSEMBLY_USAGE_OCCURRENCE('Base:1','Base:1','Base:1',#32979,#32980,
'Base:1');
#372=NEXT_ASSEMBLY_USAGE_OCCURRENCE('Foot strip:1','Foot strip:1',
'Foot strip:1',#32979,#32981,'Foot strip:1');
#373=NEXT_ASSEMBLY_USAGE_OCCURRENCE('Foot strip (1):1',
'Foot strip (1):1','Foot strip (1):1',#32979,#32982,'Foot strip (1):1');
#374=NEXT_ASSEMBLY_USAGE_OCCURRENCE('C frame:1','C frame:1','C frame:1',
#32979,#32983,'C frame:1');
#375=NEXT_ASSEMBLY_USAGE_OCCURRENCE('Split ram guide:1',
'Split ram guide:1','Split ram guide:1',#32979,#32984,
'Split ram guide:1');
#376=NEXT_ASSEMBLY_USAGE_OCCURRENCE('Guide keeper:1','Guide keeper:1',
'Guide keeper:1',#32979,#32985,'Guide keeper:1');
#377=NEXT_ASSEMBLY_USAGE_OCCURRENCE('Split ram guide (1):1',
'Split ram guide (1):1','Split ram guide (1):1',#32979,#32986,
'Split ram guide (1):1');
#378=NEXT_ASSEMBLY_USAGE_OCCURRENCE('Guide keeper (1):1',
'Guide keeper (1):1','Guide keeper (1):1',#32979,#32987,
'Guide keeper (1):1');
#379=NEXT_ASSEMBLY_USAGE_OCCURRENCE('Anvil:1','Anvil:1','Anvil:1',#32979,
#32988,'Anvil:1');
#380=NEXT_ASSEMBLY_USAGE_OCCURRENCE('Pinion bearing pedestal:1',
'Pinion bearing pedestal:1','Pinion bearing pedestal:1',#32979,#32989,
'Pinion bearing pedestal:1');
#381=NEXT_ASSEMBLY_USAGE_OCCURRENCE('Pinion bearing cap:1',
'Pinion bearing cap:1','Pinion bearing cap:1',#32979,#32990,
'Pinion bearing cap:1');
#382=NEXT_ASSEMBLY_USAGE_OCCURRENCE('Pinion bearing cap (1):1',
'Pinion bearing cap (1):1','Pinion bearing cap (1):1',#32979,#32991,
'Pinion bearing cap (1):1');
#383=NEXT_ASSEMBLY_USAGE_OCCURRENCE('Pinion bearing pedestal (1):1',
'Pinion bearing pedestal (1):1','Pinion bearing pedestal (1):1',#32979,
#32992,'Pinion bearing pedestal (1):1');
#384=NEXT_ASSEMBLY_USAGE_OCCURRENCE('Pinion bearing cap (2):1',
'Pinion bearing cap (2):1','Pinion bearing cap (2):1',#32979,#32993,
'Pinion bearing cap (2):1');
#385=NEXT_ASSEMBLY_USAGE_OCCURRENCE('Pinion bearing cap (3):1',
'Pinion bearing cap (3):1','Pinion bearing cap (3):1',#32979,#32994,
'Pinion bearing cap (3):1');
#386=NEXT_ASSEMBLY_USAGE_OCCURRENCE('Cap Screw - M5x20:2',
'Cap Screw - M5x20:2','Cap Screw - M5x20:2',#32979,#32995,
'Cap Screw - M5x20:2');
#387=NEXT_ASSEMBLY_USAGE_OCCURRENCE('Cap Screw - M5x20:3',
'Cap Screw - M5x20:3','Cap Screw - M5x20:3',#32979,#32995,
'Cap Screw - M5x20:3');
#388=NEXT_ASSEMBLY_USAGE_OCCURRENCE('Cap Screw - M5x20:4',
'Cap Screw - M5x20:4','Cap Screw - M5x20:4',#32979,#32995,
'Cap Screw - M5x20:4');
#389=NEXT_ASSEMBLY_USAGE_OCCURRENCE('Cap Screw - M5x20:5',
'Cap Screw - M5x20:5','Cap Screw - M5x20:5',#32979,#32995,
'Cap Screw - M5x20:5');
#390=NEXT_ASSEMBLY_USAGE_OCCURRENCE('M4x10 Cap Screw:2',
'M4x10 Cap Screw:2','M4x10 Cap Screw:2',#32979,#33002,
'M4x10 Cap Screw:2');
#391=NEXT_ASSEMBLY_USAGE_OCCURRENCE('M4x10 Cap Screw:3',
'M4x10 Cap Screw:3','M4x10 Cap Screw:3',#32979,#33002,
'M4x10 Cap Screw:3');
#392=NEXT_ASSEMBLY_USAGE_OCCURRENCE('M4x10 Cap Screw:4',
'M4x10 Cap Screw:4','M4x10 Cap Screw:4',#32979,#33002,
'M4x10 Cap Screw:4');
#393=NEXT_ASSEMBLY_USAGE_OCCURRENCE('M4x10 Cap Screw:5',
'M4x10 Cap Screw:5','M4x10 Cap Screw:5',#32979,#33002,
'M4x10 Cap Screw:5');
#394=NEXT_ASSEMBLY_USAGE_OCCURRENCE('M4x10 Cap Screw:6',
'M4x10 Cap Screw:6','M4x10 Cap Screw:6',#32979,#33002,
'M4x10 Cap Screw:6');
#395=NEXT_ASSEMBLY_USAGE_OCCURRENCE('M4x10 Cap Screw:7',
'M4x10 Cap Screw:7','M4x10 Cap Screw:7',#32979,#33002,
'M4x10 Cap Screw:7');
#396=NEXT_ASSEMBLY_USAGE_OCCURRENCE('Cap Screw - M4x16:2',
'Cap Screw - M4x16:2','Cap Screw - M4x16:2',#32979,#33023,
'Cap Screw - M4x16:2');
#397=NEXT_ASSEMBLY_USAGE_OCCURRENCE('Cap Screw - M4x16:3',
'Cap Screw - M4x16:3','Cap Screw - M4x16:3',#32979,#33023,
'Cap Screw - M4x16:3');
#398=NEXT_ASSEMBLY_USAGE_OCCURRENCE(
'Sealed Ball Bearing - 12 x 32 x 10 mm:2',
'Sealed Ball Bearing - 12 x 32 x 10 mm:2',
'Sealed Ball Bearing - 12 x 32 x 10 mm:2',#32979,#32996,
'Sealed Ball Bearing - 12 x 32 x 10 mm:2');
#399=NEXT_ASSEMBLY_USAGE_OCCURRENCE('M4x10 Cap Screw:8',
'M4x10 Cap Screw:8','M4x10 Cap Screw:8',#32979,#33002,
'M4x10 Cap Screw:8');
#400=NEXT_ASSEMBLY_USAGE_OCCURRENCE('M4x10 Cap Screw:9',
'M4x10 Cap Screw:9','M4x10 Cap Screw:9',#32979,#33002,
'M4x10 Cap Screw:9');
#401=NEXT_ASSEMBLY_USAGE_OCCURRENCE('M4x10 Cap Screw:10',
'M4x10 Cap Screw:10','M4x10 Cap Screw:10',#32979,#33002,
'M4x10 Cap Screw:10');
#402=NEXT_ASSEMBLY_USAGE_OCCURRENCE('M4x10 Cap Screw:11',
'M4x10 Cap Screw:11','M4x10 Cap Screw:11',#32979,#33002,
'M4x10 Cap Screw:11');
#403=NEXT_ASSEMBLY_USAGE_OCCURRENCE('M4x10 Cap Screw:12',
'M4x10 Cap Screw:12','M4x10 Cap Screw:12',#32979,#33002,
'M4x10 Cap Screw:12');
#404=NEXT_ASSEMBLY_USAGE_OCCURRENCE('M4x10 Cap Screw:13',
'M4x10 Cap Screw:13','M4x10 Cap Screw:13',#32979,#33002,
'M4x10 Cap Screw:13');
#405=NEXT_ASSEMBLY_USAGE_OCCURRENCE('M4x10 Cap Screw:14',
'M4x10 Cap Screw:14','M4x10 Cap Screw:14',#32979,#33002,
'M4x10 Cap Screw:14');
#406=NEXT_ASSEMBLY_USAGE_OCCURRENCE('M4x10 Cap Screw:15',
'M4x10 Cap Screw:15','M4x10 Cap Screw:15',#32979,#33002,
'M4x10 Cap Screw:15');
#407=NEXT_ASSEMBLY_USAGE_OCCURRENCE('Cap Screw - M4x16:4',
'Cap Screw - M4x16:4','Cap Screw - M4x16:4',#32979,#33023,
'Cap Screw - M4x16:4');
#408=NEXT_ASSEMBLY_USAGE_OCCURRENCE('Cap Screw - M4x16:5',
'Cap Screw - M4x16:5','Cap Screw - M4x16:5',#32979,#33023,
'Cap Screw - M4x16:5');
#409=NEXT_ASSEMBLY_USAGE_OCCURRENCE(
'Sealed Ball Bearing - 12 x 32 x 10 mm:3',
'Sealed Ball Bearing - 12 x 32 x 10 mm:3',
'Sealed Ball Bearing - 12 x 32 x 10 mm:3',#32979,#32996,
'Sealed Ball Bearing - 12 x 32 x 10 mm:3');
#410=NEXT_ASSEMBLY_USAGE_OCCURRENCE('M4x10 Cap Screw:16',
'M4x10 Cap Screw:16','M4x10 Cap Screw:16',#32979,#33002,
'M4x10 Cap Screw:16');
#411=NEXT_ASSEMBLY_USAGE_OCCURRENCE('M4x10 Cap Screw:17',
'M4x10 Cap Screw:17','M4x10 Cap Screw:17',#32979,#33002,
'M4x10 Cap Screw:17');
#412=NEXT_ASSEMBLY_USAGE_OCCURRENCE('M4x10 Cap Screw:18',
'M4x10 Cap Screw:18','M4x10 Cap Screw:18',#32979,#33002,
'M4x10 Cap Screw:18');
#413=NEXT_ASSEMBLY_USAGE_OCCURRENCE('M4x10 Cap Screw:19',
'M4x10 Cap Screw:19','M4x10 Cap Screw:19',#32979,#33002,
'M4x10 Cap Screw:19');
#414=NEXT_ASSEMBLY_USAGE_OCCURRENCE('M4x10 Cap Screw:20',
'M4x10 Cap Screw:20','M4x10 Cap Screw:20',#32979,#33002,
'M4x10 Cap Screw:20');
#415=NEXT_ASSEMBLY_USAGE_OCCURRENCE('M4x10 Cap Screw:21',
'M4x10 Cap Screw:21','M4x10 Cap Screw:21',#32979,#33002,
'M4x10 Cap Screw:21');
#416=NEXT_ASSEMBLY_USAGE_OCCURRENCE('M4x10 Cap Screw:22',
'M4x10 Cap Screw:22','M4x10 Cap Screw:22',#32979,#33002,
'M4x10 Cap Screw:22');
#417=NEXT_ASSEMBLY_USAGE_OCCURRENCE('M4x10 Cap Screw:23',
'M4x10 Cap Screw:23','M4x10 Cap Screw:23',#32979,#33002,
'M4x10 Cap Screw:23');
#418=NEXT_ASSEMBLY_USAGE_OCCURRENCE('Pinion shaft:1','Pinion shaft:1',
'Pinion shaft:1',#33008,#33009,'Pinion shaft:1');
#419=NEXT_ASSEMBLY_USAGE_OCCURRENCE('Inner race spacer 20 mm:1',
'Inner race spacer 20 mm:1','Inner race spacer 20 mm:1',#33008,#33010,
'Inner race spacer 20 mm:1');
#420=NEXT_ASSEMBLY_USAGE_OCCURRENCE('Inner race spacer 15 mm:1',
'Inner race spacer 15 mm:1','Inner race spacer 15 mm:1',#33008,#33011,
'Inner race spacer 15 mm:1');
#421=NEXT_ASSEMBLY_USAGE_OCCURRENCE('Inner race spacer 3 mm:1',
'Inner race spacer 3 mm:1','Inner race spacer 3 mm:1',#33008,#33012,
'Inner race spacer 3 mm:1');
#422=NEXT_ASSEMBLY_USAGE_OCCURRENCE('Inner race spacer 15 mm (1):1',
'Inner race spacer 15 mm (1):1','Inner race spacer 15 mm (1):1',#33008,
#33013,'Inner race spacer 15 mm (1):1');
#423=NEXT_ASSEMBLY_USAGE_OCCURRENCE('Parallel key 4 x 4 x 14 mm:1',
'Parallel key 4 x 4 x 14 mm:1','Parallel key 4 x 4 x 14 mm:1',#33008,#33014,
'Parallel key 4 x 4 x 14 mm:1');
#424=NEXT_ASSEMBLY_USAGE_OCCURRENCE('Parallel key 4 x 4 x 14 mm (1):1',
'Parallel key 4 x 4 x 14 mm (1):1','Parallel key 4 x 4 x 14 mm (1):1',#33008,
#33015,'Parallel key 4 x 4 x 14 mm (1):1');
#425=NEXT_ASSEMBLY_USAGE_OCCURRENCE('Operating lever:1',
'Operating lever:1','Operating lever:1',#33008,#33016,
'Operating lever:1');
#426=NEXT_ASSEMBLY_USAGE_OCCURRENCE('Handle sleeve:1','Handle sleeve:1',
'Handle sleeve:1',#33008,#33017,'Handle sleeve:1');
#427=NEXT_ASSEMBLY_USAGE_OCCURRENCE('Shaft keeper:1','Shaft keeper:1',
'Shaft keeper:1',#33008,#33018,'Shaft keeper:1');
#428=NEXT_ASSEMBLY_USAGE_OCCURRENCE('Shaft keeper (1):1',
'Shaft keeper (1):1','Shaft keeper (1):1',#33008,#33019,
'Shaft keeper (1):1');
#429=NEXT_ASSEMBLY_USAGE_OCCURRENCE(
'Spur Gear - Module 2, 20 Teeth, 12 mm Bore:2',
'Spur Gear - Module 2, 20 Teeth, 12 mm Bore:2',
'Spur Gear - Module 2, 20 Teeth, 12 mm Bore:2',#33008,#33020,
'Spur Gear - Module 2, 20 Teeth, 12 mm Bore:2');
#430=NEXT_ASSEMBLY_USAGE_OCCURRENCE('Flat Washer - M6:2',
'Flat Washer - M6:2','Flat Washer - M6:2',#33008,#33021,
'Flat Washer - M6:2');
#431=NEXT_ASSEMBLY_USAGE_OCCURRENCE('Cap Screw - M6x25:2',
'Cap Screw - M6x25:2','Cap Screw - M6x25:2',#33008,#33022,
'Cap Screw - M6x25:2');
#432=NEXT_ASSEMBLY_USAGE_OCCURRENCE('Cap Screw - M4x16:6',
'Cap Screw - M4x16:6','Cap Screw - M4x16:6',#33008,#33023,
'Cap Screw - M4x16:6');
#433=NEXT_ASSEMBLY_USAGE_OCCURRENCE('Cap Screw - M4x16:7',
'Cap Screw - M4x16:7','Cap Screw - M4x16:7',#33008,#33023,
'Cap Screw - M4x16:7');
#434=NEXT_ASSEMBLY_USAGE_OCCURRENCE('Revolving grip:1',
'Revolving grip:1','Revolving grip:1',#33024,#33025,'Revolving grip:1');
#435=NEXT_ASSEMBLY_USAGE_OCCURRENCE('Press frame and guides:1',
'Press frame and guides:1','Press frame and guides:1',#32978,#32979,
'Press frame and guides:1');
#436=NEXT_ASSEMBLY_USAGE_OCCURRENCE('Rack ram and pressure foot:1',
'Rack ram and pressure foot:1','Rack ram and pressure foot:1',#32978,#33003,
'Rack ram and pressure foot:1');
#437=NEXT_ASSEMBLY_USAGE_OCCURRENCE('Pinion and operating lever:1',
'Pinion and operating lever:1','Pinion and operating lever:1',#32978,#33008,
'Pinion and operating lever:1');
#438=NEXT_ASSEMBLY_USAGE_OCCURRENCE('Revolving hand grip:1',
'Revolving hand grip:1','Revolving hand grip:1',#32978,#33024,
'Revolving hand grip:1');
#439=B_SPLINE_CURVE_WITH_KNOTS('',3,(#18826,#18827,#18828,#18829,#18830,
#18831,#18832,#18833,#18834,#18835,#18836,#18837,#18838,#18839,#18840,#18841,
#18842,#18843,#18844,#18845,#18846,#18847),.UNSPECIFIED.,.F.,.F.,(4,2,2,
2,2,2,2,2,2,2,4),(0.0591825211272536,0.157966726598481,0.236950089897721,
0.315933453196962,0.391576304923761,0.46721915665056,0.54286200837736,0.618504860104159,
0.697488223403399,0.77647158670264,0.875255792173867),.UNSPECIFIED.);
#440=B_SPLINE_CURVE_WITH_KNOTS('',3,(#18851,#18852,#18853,#18854,#18855,
#18856,#18857,#18858,#18859,#18860,#18861,#18862,#18863,#18864,#18865,#18866,
#18867,#18868,#18869,#18870,#18871,#18872),.UNSPECIFIED.,.F.,.F.,(4,2,2,
2,2,2,2,2,2,2,4),(0.0581119756758434,0.106553146291161,0.213106292582322,
0.30849933801665,0.386091982889075,0.4636846277615,0.541277272633925,0.61886991750635,
0.714262962940678,0.820816109231839,0.869257279847157),.UNSPECIFIED.);
#441=B_SPLINE_CURVE_WITH_KNOTS('',3,(#18878,#18879,#18880,#18881,#18882,
#18883,#18884,#18885,#18886,#18887,#18888,#18889,#18890,#18891,#18892,#18893,
#18894,#18895,#18896,#18897,#18898,#18899),.UNSPECIFIED.,.F.,.F.,(4,2,2,
2,2,2,2,2,2,2,4),(0.0581119756758434,0.106553146291161,0.213106292582322,
0.30849933801665,0.386091982889075,0.4636846277615,0.541277272633925,0.61886991750635,
0.714262962940679,0.820816109231839,0.869257279847157),.UNSPECIFIED.);
#442=B_SPLINE_CURVE_WITH_KNOTS('',3,(#18903,#18904,#18905,#18906,#18907,
#18908,#18909,#18910,#18911,#18912,#18913,#18914,#18915,#18916,#18917,#18918,
#18919,#18920,#18921,#18922,#18923,#18924),.UNSPECIFIED.,.F.,.F.,(4,2,2,
2,2,2,2,2,2,2,4),(0.0581119756758433,0.106553146291161,0.213106292582322,
0.308499338016649,0.386091982889075,0.4636846277615,0.541277272633925,0.61886991750635,
0.714262962940678,0.820816109231839,0.869257279847157),.UNSPECIFIED.);
#443=B_SPLINE_CURVE_WITH_KNOTS('',3,(#18933,#18934,#18935,#18936,#18937,
#18938,#18939,#18940,#18941,#18942,#18943,#18944,#18945,#18946,#18947,#18948,
#18949,#18950,#18951,#18952,#18953,#18954),.UNSPECIFIED.,.F.,.F.,(4,2,2,
2,2,2,2,2,2,2,4),(0.0581119756758433,0.106553146291161,0.213106292582322,
0.30849933801665,0.386091982889075,0.4636846277615,0.541277272633925,0.61886991750635,
0.714262962940678,0.820816109231839,0.869257279847157),.UNSPECIFIED.);
#444=B_SPLINE_CURVE_WITH_KNOTS('',3,(#18958,#18959,#18960,#18961,#18962,
#18963,#18964,#18965,#18966,#18967,#18968,#18969,#18970,#18971,#18972,#18973,
#18974,#18975,#18976,#18977,#18978,#18979),.UNSPECIFIED.,.F.,.F.,(4,2,2,
2,2,2,2,2,2,2,4),(0.0581119756758434,0.106553146291161,0.213106292582322,
0.30849933801665,0.386091982889075,0.4636846277615,0.541277272633925,0.61886991750635,
0.714262962940678,0.820816109231839,0.869257279847157),.UNSPECIFIED.);
#445=B_SPLINE_CURVE_WITH_KNOTS('',3,(#18983,#18984,#18985,#18986,#18987,
#18988,#18989,#18990,#18991,#18992,#18993,#18994,#18995,#18996,#18997,#18998,
#18999,#19000,#19001,#19002,#19003,#19004),.UNSPECIFIED.,.F.,.F.,(4,2,2,
2,2,2,2,2,2,2,4),(0.0581119756758434,0.106553146291161,0.213106292582322,
0.30849933801665,0.386091982889075,0.4636846277615,0.541277272633925,0.61886991750635,
0.714262962940678,0.820816109231839,0.869257279847157),.UNSPECIFIED.);
#446=B_SPLINE_CURVE_WITH_KNOTS('',3,(#19008,#19009,#19010,#19011,#19012,
#19013,#19014,#19015,#19016,#19017,#19018,#19019,#19020,#19021,#19022,#19023,
#19024,#19025,#19026,#19027,#19028,#19029),.UNSPECIFIED.,.F.,.F.,(4,2,2,
2,2,2,2,2,2,2,4),(0.0581119756758433,0.106553146291161,0.213106292582322,
0.30849933801665,0.386091982889075,0.4636846277615,0.541277272633925,0.61886991750635,
0.714262962940678,0.820816109231839,0.869257279847157),.UNSPECIFIED.);
#447=B_SPLINE_CURVE_WITH_KNOTS('',3,(#19037,#19038,#19039,#19040,#19041,
#19042,#19043,#19044,#19045,#19046,#19047,#19048,#19049,#19050,#19051,#19052,
#19053,#19054,#19055,#19056,#19057,#19058),.UNSPECIFIED.,.F.,.F.,(4,2,2,
2,2,2,2,2,2,2,4),(0.0591825211272536,0.157966726598481,0.236950089897721,
0.315933453196962,0.391576304923761,0.467219156650561,0.54286200837736,
0.618504860104159,0.697488223403399,0.77647158670264,0.875255792173867),
 .UNSPECIFIED.);
#448=B_SPLINE_CURVE_WITH_KNOTS('',3,(#19066,#19067,#19068,#19069,#19070,
#19071,#19072,#19073,#19074,#19075,#19076,#19077,#19078,#19079,#19080,#19081,
#19082,#19083,#19084,#19085,#19086,#19087),.UNSPECIFIED.,.F.,.F.,(4,2,2,
2,2,2,2,2,2,2,4),(0.0591825211272536,0.157966726598481,0.236950089897722,
0.315933453196962,0.391576304923761,0.467219156650561,0.54286200837736,
0.618504860104159,0.697488223403399,0.77647158670264,0.875255792173867),
 .UNSPECIFIED.);
#449=B_SPLINE_CURVE_WITH_KNOTS('',3,(#19097,#19098,#19099,#19100,#19101,
#19102,#19103,#19104,#19105,#19106,#19107,#19108,#19109,#19110,#19111,#19112,
#19113,#19114,#19115,#19116,#19117,#19118),.UNSPECIFIED.,.F.,.F.,(4,2,2,
2,2,2,2,2,2,2,4),(0.0591825211272536,0.157966726598481,0.236950089897721,
0.315933453196962,0.391576304923761,0.46721915665056,0.54286200837736,0.618504860104159,
0.697488223403399,0.77647158670264,0.875255792173867),.UNSPECIFIED.);
#450=B_SPLINE_CURVE_WITH_KNOTS('',3,(#19126,#19127,#19128,#19129,#19130,
#19131,#19132,#19133,#19134,#19135,#19136,#19137,#19138,#19139,#19140,#19141,
#19142,#19143,#19144,#19145,#19146,#19147),.UNSPECIFIED.,.F.,.F.,(4,2,2,
2,2,2,2,2,2,2,4),(0.0591825211272536,0.157966726598481,0.236950089897721,
0.315933453196962,0.391576304923761,0.46721915665056,0.542862008377359,
0.618504860104159,0.697488223403399,0.776471586702639,0.875255792173867),
 .UNSPECIFIED.);
#451=B_SPLINE_CURVE_WITH_KNOTS('',3,(#19155,#19156,#19157,#19158,#19159,
#19160,#19161,#19162,#19163,#19164,#19165,#19166,#19167,#19168,#19169,#19170,
#19171,#19172,#19173,#19174,#19175,#19176),.UNSPECIFIED.,.F.,.F.,(4,2,2,
2,2,2,2,2,2,2,4),(0.0591825211272536,0.157966726598481,0.236950089897721,
0.315933453196962,0.391576304923761,0.46721915665056,0.54286200837736,0.618504860104159,
0.697488223403399,0.77647158670264,0.875255792173867),.UNSPECIFIED.);
#452=B_SPLINE_CURVE_WITH_KNOTS('',3,(#19185,#19186,#19187,#19188,#19189,
#19190,#19191,#19192,#19193,#19194,#19195,#19196,#19197,#19198,#19199,#19200,
#19201,#19202,#19203,#19204,#19205,#19206),.UNSPECIFIED.,.F.,.F.,(4,2,2,
2,2,2,2,2,2,2,4),(0.0591825211272536,0.157966726598481,0.236950089897721,
0.315933453196962,0.391576304923761,0.46721915665056,0.542862008377359,
0.618504860104159,0.697488223403399,0.776471586702639,0.875255792173867),
 .UNSPECIFIED.);
#453=B_SPLINE_CURVE_WITH_KNOTS('',3,(#20353,#20354,#20355,#20356,#20357,
#20358,#20359,#20360,#20361,#20362),.UNSPECIFIED.,.F.,.F.,(4,2,2,2,4),(0.,
0.0622753849594643,0.124550769918929,0.186824589898795,0.249098409878661),
 .UNSPECIFIED.);
#454=B_SPLINE_CURVE_WITH_KNOTS('',3,(#20363,#20364,#20365,#20366,#20367,
#20368,#20369,#20370,#20371,#20372,#20373,#20374,#20375,#20376,#20377,#20378,
#20379,#20380,#20381,#20382,#20383,#20384,#20385,#20386,#20387,#20388),
 .UNSPECIFIED.,.F.,.F.,(4,2,2,2,2,2,2,2,2,2,2,2,4),(0.249098409878661,0.311372229858528,
0.373646049838394,0.435921434797858,0.498196819757323,0.560472204716787,
0.622747589676251,0.685021409656117,0.747295229635984,0.80956904961585,
0.871842869595717,0.934118254555181,0.996393639514645),.UNSPECIFIED.);
#455=B_SPLINE_CURVE_WITH_KNOTS('',3,(#20392,#20393,#20394,#20395,#20396,
#20397,#20398,#20399,#20400,#20401,#20402,#20403,#20404,#20405,#20406,#20407,
#20408,#20409,#20410,#20411,#20412,#20413,#20414,#20415,#20416,#20417),
 .UNSPECIFIED.,.F.,.F.,(4,2,2,2,2,2,2,2,2,2,2,2,4),(0.,0.0621954302022346,
0.124390860404469,0.186586102839082,0.248781345273694,0.310976587708307,
0.37317183014292,0.435367260345154,0.497562690547389,0.559758120749623,
0.621953550951858,0.68414879338647,0.746344035821083),.UNSPECIFIED.);
#456=B_SPLINE_CURVE_WITH_KNOTS('',3,(#20418,#20419,#20420,#20421,#20422,
#20423,#20424,#20425,#20426,#20427),.UNSPECIFIED.,.F.,.F.,(4,2,2,2,4),(0.746344035821083,
0.808539278255696,0.870734520690308,0.932929950892543,0.995125381094778),
 .UNSPECIFIED.);
#457=SPHERICAL_SURFACE('',#13456,0.29765);
#458=SPHERICAL_SURFACE('',#13458,0.29765);
#459=SPHERICAL_SURFACE('',#13460,0.29765);
#460=SPHERICAL_SURFACE('',#13462,0.29765);
#461=SPHERICAL_SURFACE('',#13464,0.29765);
#462=SPHERICAL_SURFACE('',#13466,0.29765);
#463=SPHERICAL_SURFACE('',#13468,0.29765);
#464=SPHERICAL_SURFACE('',#13471,0.309556);
#465=SPHERICAL_SURFACE('',#13487,0.309556);
#466=SPHERICAL_SURFACE('',#13492,0.309556);
#467=SPHERICAL_SURFACE('',#13498,0.309556);
#468=SPHERICAL_SURFACE('',#13503,0.309556);
#469=SPHERICAL_SURFACE('',#13508,0.309556);
#470=SPHERICAL_SURFACE('',#13516,0.309556);
#471=TOROIDAL_SURFACE('',#13416,1.1,0.309556);
#472=TOROIDAL_SURFACE('',#13436,1.1,0.309556);
#473=ORIENTED_CLOSED_SHELL('',*,#12499,.F.);
#474=ORIENTED_CLOSED_SHELL('',*,#12512,.F.);
#475=ORIENTED_CLOSED_SHELL('',*,#12532,.F.);
#476=ORIENTED_CLOSED_SHELL('',*,#12534,.F.);
#477=CONICAL_SURFACE('',#13391,0.4,0.785398163397448);
#478=CONICAL_SURFACE('',#13395,0.41,0.785398163397448);
#479=CONICAL_SURFACE('',#13399,0.26,0.463647609000806);
#480=CONICAL_SURFACE('',#13403,0.225,0.785398163397448);
#481=CONICAL_SURFACE('',#13427,0.63,0.785398163397448);
#482=CONICAL_SURFACE('',#13434,0.63,0.785398163397448);
#483=CONICAL_SURFACE('',#13447,1.57,0.785398163397449);
#484=CONICAL_SURFACE('',#13451,1.57,0.785398163397449);
#485=CONICAL_SURFACE('',#13555,0.325,0.785398163397448);
#486=CONICAL_SURFACE('',#13559,0.335,0.785398163397448);
#487=CONICAL_SURFACE('',#13563,0.21,0.463647609000806);
#488=CONICAL_SURFACE('',#13782,0.185,0.785398163397449);
#489=CONICAL_SURFACE('',#13786,0.1625,0.785398163397449);
#490=CONICAL_SURFACE('',#14028,0.475,0.785398163397449);
#491=CONICAL_SURFACE('',#14032,0.485,0.785398163397448);
#492=CONICAL_SURFACE('',#14036,0.31,0.463647609000806);
#493=CONICAL_SURFACE('',#14040,0.27,0.785398163397448);
#494=CONICAL_SURFACE('',#14054,0.325,0.785398163397448);
#495=CONICAL_SURFACE('',#14058,0.335,0.785398163397448);
#496=CONICAL_SURFACE('',#14062,0.21,0.463647609000806);
#497=CONICAL_SURFACE('',#14066,0.18,0.785398163397448);
#498=BREP_WITH_VOIDS('Body1',#12498,(#473));
#499=BREP_WITH_VOIDS('Body1',#12513,(#474));
#500=BREP_WITH_VOIDS('Body1',#12531,(#475));
#501=BREP_WITH_VOIDS('Body1',#12533,(#476));
#502=SHAPE_REPRESENTATION_RELATIONSHIP('SRR','None',#32931,#544);
#503=SHAPE_REPRESENTATION_RELATIONSHIP('SRR','None',#32932,#545);
#504=SHAPE_REPRESENTATION_RELATIONSHIP('SRR','None',#32933,#546);
#505=SHAPE_REPRESENTATION_RELATIONSHIP('SRR','None',#32934,#547);
#506=SHAPE_REPRESENTATION_RELATIONSHIP('SRR','None',#32935,#548);
#507=SHAPE_REPRESENTATION_RELATIONSHIP('SRR','None',#32936,#549);
#508=SHAPE_REPRESENTATION_RELATIONSHIP('SRR','None',#32937,#550);
#509=SHAPE_REPRESENTATION_RELATIONSHIP('SRR','None',#32938,#551);
#510=SHAPE_REPRESENTATION_RELATIONSHIP('SRR','None',#32939,#552);
#511=SHAPE_REPRESENTATION_RELATIONSHIP('SRR','None',#32940,#553);
#512=SHAPE_REPRESENTATION_RELATIONSHIP('SRR','None',#32941,#554);
#513=SHAPE_REPRESENTATION_RELATIONSHIP('SRR','None',#32942,#555);
#514=SHAPE_REPRESENTATION_RELATIONSHIP('SRR','None',#32943,#556);
#515=SHAPE_REPRESENTATION_RELATIONSHIP('SRR','None',#32944,#557);
#516=SHAPE_REPRESENTATION_RELATIONSHIP('SRR','None',#32945,#558);
#517=SHAPE_REPRESENTATION_RELATIONSHIP('SRR','None',#32946,#559);
#518=SHAPE_REPRESENTATION_RELATIONSHIP('SRR','None',#32948,#560);
#519=SHAPE_REPRESENTATION_RELATIONSHIP('SRR','None',#32949,#561);
#520=SHAPE_REPRESENTATION_RELATIONSHIP('SRR','None',#32950,#562);
#521=SHAPE_REPRESENTATION_RELATIONSHIP('SRR','None',#32951,#563);
#522=SHAPE_REPRESENTATION_RELATIONSHIP('SRR','None',#32952,#564);
#523=SHAPE_REPRESENTATION_RELATIONSHIP('SRR','None',#32953,#565);
#524=SHAPE_REPRESENTATION_RELATIONSHIP('SRR','None',#32955,#566);
#525=SHAPE_REPRESENTATION_RELATIONSHIP('SRR','None',#32956,#567);
#526=SHAPE_REPRESENTATION_RELATIONSHIP('SRR','None',#32957,#568);
#527=SHAPE_REPRESENTATION_RELATIONSHIP('SRR','None',#32958,#569);
#528=SHAPE_REPRESENTATION_RELATIONSHIP('SRR','None',#32960,#570);
#529=SHAPE_REPRESENTATION_RELATIONSHIP('SRR','None',#32961,#571);
#530=SHAPE_REPRESENTATION_RELATIONSHIP('SRR','None',#32962,#572);
#531=SHAPE_REPRESENTATION_RELATIONSHIP('SRR','None',#32963,#573);
#532=SHAPE_REPRESENTATION_RELATIONSHIP('SRR','None',#32964,#574);
#533=SHAPE_REPRESENTATION_RELATIONSHIP('SRR','None',#32965,#575);
#534=SHAPE_REPRESENTATION_RELATIONSHIP('SRR','None',#32966,#576);
#535=SHAPE_REPRESENTATION_RELATIONSHIP('SRR','None',#32967,#577);
#536=SHAPE_REPRESENTATION_RELATIONSHIP('SRR','None',#32968,#578);
#537=SHAPE_REPRESENTATION_RELATIONSHIP('SRR','None',#32969,#579);
#538=SHAPE_REPRESENTATION_RELATIONSHIP('SRR','None',#32970,#580);
#539=SHAPE_REPRESENTATION_RELATIONSHIP('SRR','None',#32971,#581);
#540=SHAPE_REPRESENTATION_RELATIONSHIP('SRR','None',#32972,#582);
#541=SHAPE_REPRESENTATION_RELATIONSHIP('SRR','None',#32973,#583);
#542=SHAPE_REPRESENTATION_RELATIONSHIP('SRR','None',#32974,#584);
#543=SHAPE_REPRESENTATION_RELATIONSHIP('SRR','None',#32976,#585);
#544=ADVANCED_BREP_SHAPE_REPRESENTATION('',(#635),#32705);
#545=ADVANCED_BREP_SHAPE_REPRESENTATION('',(#636),#32706);
#546=ADVANCED_BREP_SHAPE_REPRESENTATION('',(#637),#32707);
#547=ADVANCED_BREP_SHAPE_REPRESENTATION('',(#638),#32708);
#548=ADVANCED_BREP_SHAPE_REPRESENTATION('',(#639),#32709);
#549=ADVANCED_BREP_SHAPE_REPRESENTATION('',(#640),#32710);
#550=ADVANCED_BREP_SHAPE_REPRESENTATION('',(#641),#32711);
#551=ADVANCED_BREP_SHAPE_REPRESENTATION('',(#642),#32712);
#552=ADVANCED_BREP_SHAPE_REPRESENTATION('',(#643),#32713);
#553=ADVANCED_BREP_SHAPE_REPRESENTATION('',(#644),#32714);
#554=ADVANCED_BREP_SHAPE_REPRESENTATION('',(#645),#32715);
#555=ADVANCED_BREP_SHAPE_REPRESENTATION('',(#646),#32716);
#556=ADVANCED_BREP_SHAPE_REPRESENTATION('',(#647),#32717);
#557=ADVANCED_BREP_SHAPE_REPRESENTATION('',(#648),#32718);
#558=ADVANCED_BREP_SHAPE_REPRESENTATION('',(#649),#32719);
#559=ADVANCED_BREP_SHAPE_REPRESENTATION('',(#498),#32720);
#560=ADVANCED_BREP_SHAPE_REPRESENTATION('',(#650),#32722);
#561=ADVANCED_BREP_SHAPE_REPRESENTATION('',(#651),#32723);
#562=ADVANCED_BREP_SHAPE_REPRESENTATION('',(#652,#653,#654,#655,#656,#657,
#658),#32724);
#563=ADVANCED_BREP_SHAPE_REPRESENTATION('',(#659),#32725);
#564=ADVANCED_BREP_SHAPE_REPRESENTATION('',(#660,#661),#32726);
#565=ADVANCED_BREP_SHAPE_REPRESENTATION('',(#499),#32727);
#566=ADVANCED_BREP_SHAPE_REPRESENTATION('',(#662),#32729);
#567=ADVANCED_BREP_SHAPE_REPRESENTATION('',(#663),#32730);
#568=ADVANCED_BREP_SHAPE_REPRESENTATION('',(#664),#32731);
#569=ADVANCED_BREP_SHAPE_REPRESENTATION('',(#665),#32732);
#570=ADVANCED_BREP_SHAPE_REPRESENTATION('',(#666),#32734);
#571=ADVANCED_BREP_SHAPE_REPRESENTATION('',(#667),#32735);
#572=ADVANCED_BREP_SHAPE_REPRESENTATION('',(#668),#32736);
#573=ADVANCED_BREP_SHAPE_REPRESENTATION('',(#669),#32737);
#574=ADVANCED_BREP_SHAPE_REPRESENTATION('',(#670),#32738);
#575=ADVANCED_BREP_SHAPE_REPRESENTATION('',(#671),#32739);
#576=ADVANCED_BREP_SHAPE_REPRESENTATION('',(#672),#32740);
#577=ADVANCED_BREP_SHAPE_REPRESENTATION('',(#673),#32741);
#578=ADVANCED_BREP_SHAPE_REPRESENTATION('',(#674),#32742);
#579=ADVANCED_BREP_SHAPE_REPRESENTATION('',(#675),#32743);
#580=ADVANCED_BREP_SHAPE_REPRESENTATION('',(#676),#32744);
#581=ADVANCED_BREP_SHAPE_REPRESENTATION('',(#677),#32745);
#582=ADVANCED_BREP_SHAPE_REPRESENTATION('',(#678),#32746);
#583=ADVANCED_BREP_SHAPE_REPRESENTATION('',(#500),#32747);
#584=ADVANCED_BREP_SHAPE_REPRESENTATION('',(#501),#32748);
#585=ADVANCED_BREP_SHAPE_REPRESENTATION('',(#679),#32750);
#586=STYLED_ITEM('',(#33221),#635);
#587=STYLED_ITEM('',(#33228),#636);
#588=STYLED_ITEM('',(#33228),#637);
#589=STYLED_ITEM('',(#33221),#638);
#590=STYLED_ITEM('',(#33235),#639);
#591=STYLED_ITEM('',(#33235),#640);
#592=STYLED_ITEM('',(#33235),#641);
#593=STYLED_ITEM('',(#33235),#642);
#594=STYLED_ITEM('',(#33235),#643);
#595=STYLED_ITEM('',(#33242),#644);
#596=STYLED_ITEM('',(#33242),#645);
#597=STYLED_ITEM('',(#33242),#646);
#598=STYLED_ITEM('',(#33242),#647);
#599=STYLED_ITEM('',(#33242),#648);
#600=STYLED_ITEM('',(#33242),#649);
#601=STYLED_ITEM('',(#33249),#498);
#602=STYLED_ITEM('',(#33242),#650);
#603=STYLED_ITEM('',(#33242),#651);
#604=STYLED_ITEM('',(#33242),#652);
#605=STYLED_ITEM('',(#33242),#653);
#606=STYLED_ITEM('',(#33242),#654);
#607=STYLED_ITEM('',(#33242),#655);
#608=STYLED_ITEM('',(#33242),#656);
#609=STYLED_ITEM('',(#33242),#657);
#610=STYLED_ITEM('',(#33242),#658);
#611=STYLED_ITEM('',(#33242),#659);
#612=STYLED_ITEM('',(#33242),#660);
#613=STYLED_ITEM('',(#33242),#661);
#614=STYLED_ITEM('',(#33249),#499);
#615=STYLED_ITEM('',(#33228),#662);
#616=STYLED_ITEM('',(#33256),#663);
#617=STYLED_ITEM('',(#33228),#664);
#618=STYLED_ITEM('',(#33249),#665);
#619=STYLED_ITEM('',(#33242),#666);
#620=STYLED_ITEM('',(#33242),#667);
#621=STYLED_ITEM('',(#33242),#668);
#622=STYLED_ITEM('',(#33242),#669);
#623=STYLED_ITEM('',(#33242),#670);
#624=STYLED_ITEM('',(#33242),#671);
#625=STYLED_ITEM('',(#33242),#672);
#626=STYLED_ITEM('',(#33228),#673);
#627=STYLED_ITEM('',(#33256),#674);
#628=STYLED_ITEM('',(#33242),#675);
#629=STYLED_ITEM('',(#33242),#676);
#630=STYLED_ITEM('',(#33256),#677);
#631=STYLED_ITEM('',(#33249),#678);
#632=STYLED_ITEM('',(#33249),#500);
#633=STYLED_ITEM('',(#33249),#501);
#634=STYLED_ITEM('',(#33249),#679);
#635=MANIFOLD_SOLID_BREP('Body1',#12483);
#636=MANIFOLD_SOLID_BREP('Body1',#12484);
#637=MANIFOLD_SOLID_BREP('Body1',#12485);
#638=MANIFOLD_SOLID_BREP('Body1',#12486);
#639=MANIFOLD_SOLID_BREP('Body1',#12487);
#640=MANIFOLD_SOLID_BREP('Body1',#12488);
#641=MANIFOLD_SOLID_BREP('Body1',#12489);
#642=MANIFOLD_SOLID_BREP('Body1',#12490);
#643=MANIFOLD_SOLID_BREP('Body1',#12491);
#644=MANIFOLD_SOLID_BREP('Body1',#12492);
#645=MANIFOLD_SOLID_BREP('Body1',#12493);
#646=MANIFOLD_SOLID_BREP('Body1',#12494);
#647=MANIFOLD_SOLID_BREP('Body1',#12495);
#648=MANIFOLD_SOLID_BREP('Body1',#12496);
#649=MANIFOLD_SOLID_BREP('Body1',#12497);
#650=MANIFOLD_SOLID_BREP('Body1',#12500);
#651=MANIFOLD_SOLID_BREP('Body1',#12501);
#652=MANIFOLD_SOLID_BREP('Body1',#12502);
#653=MANIFOLD_SOLID_BREP('Body2',#12503);
#654=MANIFOLD_SOLID_BREP('Body3',#12504);
#655=MANIFOLD_SOLID_BREP('Body4',#12505);
#656=MANIFOLD_SOLID_BREP('Body5',#12506);
#657=MANIFOLD_SOLID_BREP('Body6',#12507);
#658=MANIFOLD_SOLID_BREP('Body7',#12508);
#659=MANIFOLD_SOLID_BREP('Continuous crown cage',#12509);
#660=MANIFOLD_SOLID_BREP('Body1',#12510);
#661=MANIFOLD_SOLID_BREP('Body2',#12511);
#662=MANIFOLD_SOLID_BREP('Body1',#12514);
#663=MANIFOLD_SOLID_BREP('Body1',#12515);
#664=MANIFOLD_SOLID_BREP('Body1',#12516);
#665=MANIFOLD_SOLID_BREP('Body1',#12517);
#666=MANIFOLD_SOLID_BREP('Body1',#12518);
#667=MANIFOLD_SOLID_BREP('Body1',#12519);
#668=MANIFOLD_SOLID_BREP('Body1',#12520);
#669=MANIFOLD_SOLID_BREP('Body1',#12521);
#670=MANIFOLD_SOLID_BREP('Body1',#12522);
#671=MANIFOLD_SOLID_BREP('Body1',#12523);
#672=MANIFOLD_SOLID_BREP('Body1',#12524);
#673=MANIFOLD_SOLID_BREP('Body1',#12525);
#674=MANIFOLD_SOLID_BREP('Body1',#12526);
#675=MANIFOLD_SOLID_BREP('Body1',#12527);
#676=MANIFOLD_SOLID_BREP('Body1',#12528);
#677=MANIFOLD_SOLID_BREP('Body1',#12529);
#678=MANIFOLD_SOLID_BREP('Body1',#12530);
#679=MANIFOLD_SOLID_BREP('Body1',#12535);
#680=FACE_BOUND('',#1989,.T.);
#681=FACE_BOUND('',#1990,.T.);
#682=FACE_BOUND('',#1991,.T.);
#683=FACE_BOUND('',#1992,.T.);
#684=FACE_BOUND('',#1993,.T.);
#685=FACE_BOUND('',#1994,.T.);
#686=FACE_BOUND('',#1995,.T.);
#687=FACE_BOUND('',#1996,.T.);
#688=FACE_BOUND('',#1997,.T.);
#689=FACE_BOUND('',#1998,.T.);
#690=FACE_BOUND('',#2000,.T.);
#691=FACE_BOUND('',#2001,.T.);
#692=FACE_BOUND('',#2002,.T.);
#693=FACE_BOUND('',#2003,.T.);
#694=FACE_BOUND('',#2004,.T.);
#695=FACE_BOUND('',#2005,.T.);
#696=FACE_BOUND('',#2006,.T.);
#697=FACE_BOUND('',#2007,.T.);
#698=FACE_BOUND('',#2008,.T.);
#699=FACE_BOUND('',#2009,.T.);
#700=FACE_BOUND('',#2033,.T.);
#701=FACE_BOUND('',#2034,.T.);
#702=FACE_BOUND('',#2048,.T.);
#703=FACE_BOUND('',#2049,.T.);
#704=FACE_BOUND('',#2057,.T.);
#705=FACE_BOUND('',#2058,.T.);
#706=FACE_BOUND('',#2059,.T.);
#707=FACE_BOUND('',#2060,.T.);
#708=FACE_BOUND('',#2061,.T.);
#709=FACE_BOUND('',#2070,.T.);
#710=FACE_BOUND('',#2071,.T.);
#711=FACE_BOUND('',#2074,.T.);
#712=FACE_BOUND('',#2075,.T.);
#713=FACE_BOUND('',#2076,.T.);
#714=FACE_BOUND('',#2077,.T.);
#715=FACE_BOUND('',#2097,.T.);
#716=FACE_BOUND('',#2098,.T.);
#717=FACE_BOUND('',#2104,.T.);
#718=FACE_BOUND('',#2105,.T.);
#719=FACE_BOUND('',#2125,.T.);
#720=FACE_BOUND('',#2126,.T.);
#721=FACE_BOUND('',#2132,.T.);
#722=FACE_BOUND('',#2133,.T.);
#723=FACE_BOUND('',#2136,.T.);
#724=FACE_BOUND('',#2139,.T.);
#725=FACE_BOUND('',#2144,.T.);
#726=FACE_BOUND('',#2145,.T.);
#727=FACE_BOUND('',#2147,.T.);
#728=FACE_BOUND('',#2148,.T.);
#729=FACE_BOUND('',#2151,.T.);
#730=FACE_BOUND('',#2152,.T.);
#731=FACE_BOUND('',#2162,.T.);
#732=FACE_BOUND('',#2164,.T.);
#733=FACE_BOUND('',#2167,.T.);
#734=FACE_BOUND('',#2168,.T.);
#735=FACE_BOUND('',#2169,.T.);
#736=FACE_BOUND('',#2170,.T.);
#737=FACE_BOUND('',#2171,.T.);
#738=FACE_BOUND('',#2174,.T.);
#739=FACE_BOUND('',#2175,.T.);
#740=FACE_BOUND('',#2176,.T.);
#741=FACE_BOUND('',#2177,.T.);
#742=FACE_BOUND('',#2178,.T.);
#743=FACE_BOUND('',#2188,.T.);
#744=FACE_BOUND('',#2191,.T.);
#745=FACE_BOUND('',#2192,.T.);
#746=FACE_BOUND('',#2193,.T.);
#747=FACE_BOUND('',#2194,.T.);
#748=FACE_BOUND('',#2195,.T.);
#749=FACE_BOUND('',#2197,.T.);
#750=FACE_BOUND('',#2198,.T.);
#751=FACE_BOUND('',#2199,.T.);
#752=FACE_BOUND('',#2200,.T.);
#753=FACE_BOUND('',#2201,.T.);
#754=FACE_BOUND('',#2209,.T.);
#755=FACE_BOUND('',#2212,.T.);
#756=FACE_BOUND('',#2213,.T.);
#757=FACE_BOUND('',#2214,.T.);
#758=FACE_BOUND('',#2215,.T.);
#759=FACE_BOUND('',#2216,.T.);
#760=FACE_BOUND('',#2218,.T.);
#761=FACE_BOUND('',#2219,.T.);
#762=FACE_BOUND('',#2220,.T.);
#763=FACE_BOUND('',#2221,.T.);
#764=FACE_BOUND('',#2222,.T.);
#765=FACE_BOUND('',#2225,.T.);
#766=FACE_BOUND('',#2226,.T.);
#767=FACE_BOUND('',#2228,.T.);
#768=FACE_BOUND('',#2229,.T.);
#769=FACE_BOUND('',#2230,.T.);
#770=FACE_BOUND('',#2231,.T.);
#771=FACE_BOUND('',#2232,.T.);
#772=FACE_BOUND('',#2241,.T.);
#773=FACE_BOUND('',#2243,.T.);
#774=FACE_BOUND('',#2248,.T.);
#775=FACE_BOUND('',#2249,.T.);
#776=FACE_BOUND('',#2250,.T.);
#777=FACE_BOUND('',#2251,.T.);
#778=FACE_BOUND('',#2252,.T.);
#779=FACE_BOUND('',#2262,.T.);
#780=FACE_BOUND('',#2265,.T.);
#781=FACE_BOUND('',#2266,.T.);
#782=FACE_BOUND('',#2267,.T.);
#783=FACE_BOUND('',#2268,.T.);
#784=FACE_BOUND('',#2269,.T.);
#785=FACE_BOUND('',#2271,.T.);
#786=FACE_BOUND('',#2272,.T.);
#787=FACE_BOUND('',#2273,.T.);
#788=FACE_BOUND('',#2274,.T.);
#789=FACE_BOUND('',#2275,.T.);
#790=FACE_BOUND('',#2283,.T.);
#791=FACE_BOUND('',#2286,.T.);
#792=FACE_BOUND('',#2287,.T.);
#793=FACE_BOUND('',#2288,.T.);
#794=FACE_BOUND('',#2289,.T.);
#795=FACE_BOUND('',#2290,.T.);
#796=FACE_BOUND('',#2292,.T.);
#797=FACE_BOUND('',#2293,.T.);
#798=FACE_BOUND('',#2294,.T.);
#799=FACE_BOUND('',#2295,.T.);
#800=FACE_BOUND('',#2296,.T.);
#801=FACE_BOUND('',#2302,.T.);
#802=FACE_BOUND('',#2320,.T.);
#803=FACE_BOUND('',#2323,.T.);
#804=FACE_BOUND('',#2328,.T.);
#805=FACE_BOUND('',#2333,.T.);
#806=FACE_BOUND('',#2358,.T.);
#807=FACE_BOUND('',#2361,.T.);
#808=FACE_BOUND('',#2364,.T.);
#809=FACE_BOUND('',#2367,.T.);
#810=FACE_BOUND('',#2370,.T.);
#811=FACE_BOUND('',#2386,.T.);
#812=FACE_BOUND('',#2561,.T.);
#813=FACE_BOUND('',#2566,.T.);
#814=FACE_BOUND('',#2575,.T.);
#815=FACE_BOUND('',#2577,.T.);
#816=FACE_BOUND('',#2587,.T.);
#817=FACE_BOUND('',#2607,.T.);
#818=FACE_BOUND('',#2608,.T.);
#819=FACE_BOUND('',#2610,.T.);
#820=FACE_BOUND('',#2612,.T.);
#821=FACE_BOUND('',#2616,.T.);
#822=FACE_BOUND('',#2618,.T.);
#823=FACE_BOUND('',#2622,.T.);
#824=FACE_BOUND('',#2624,.T.);
#825=FACE_BOUND('',#2628,.T.);
#826=FACE_BOUND('',#2630,.T.);
#827=FACE_BOUND('',#2634,.T.);
#828=FACE_BOUND('',#2636,.T.);
#829=FACE_BOUND('',#2654,.T.);
#830=FACE_BOUND('',#2659,.T.);
#831=FACE_BOUND('',#2662,.T.);
#832=FACE_BOUND('',#2664,.T.);
#833=FACE_BOUND('',#2666,.T.);
#834=FACE_BOUND('',#2670,.T.);
#835=FACE_BOUND('',#2672,.T.);
#836=FACE_BOUND('',#2676,.T.);
#837=FACE_BOUND('',#2678,.T.);
#838=FACE_BOUND('',#2682,.T.);
#839=FACE_BOUND('',#2684,.T.);
#840=FACE_BOUND('',#2689,.T.);
#841=FACE_BOUND('',#2693,.T.);
#842=FACE_BOUND('',#2774,.T.);
#843=FACE_BOUND('',#2779,.T.);
#844=FACE_BOUND('',#2781,.T.);
#845=FACE_BOUND('',#2787,.T.);
#846=FACE_BOUND('',#2805,.T.);
#847=FACE_BOUND('',#2821,.T.);
#848=FACE_BOUND('',#2823,.T.);
#849=PLANE('',#13032);
#850=PLANE('',#13033);
#851=PLANE('',#13034);
#852=PLANE('',#13035);
#853=PLANE('',#13036);
#854=PLANE('',#13037);
#855=PLANE('',#13039);
#856=PLANE('',#13040);
#857=PLANE('',#13041);
#858=PLANE('',#13042);
#859=PLANE('',#13043);
#860=PLANE('',#13044);
#861=PLANE('',#13046);
#862=PLANE('',#13047);
#863=PLANE('',#13048);
#864=PLANE('',#13049);
#865=PLANE('',#13050);
#866=PLANE('',#13051);
#867=PLANE('',#13056);
#868=PLANE('',#13060);
#869=PLANE('',#13061);
#870=PLANE('',#13062);
#871=PLANE('',#13063);
#872=PLANE('',#13073);
#873=PLANE('',#13074);
#874=PLANE('',#13075);
#875=PLANE('',#13079);
#876=PLANE('',#13083);
#877=PLANE('',#13084);
#878=PLANE('',#13085);
#879=PLANE('',#13086);
#880=PLANE('',#13096);
#881=PLANE('',#13097);
#882=PLANE('',#13098);
#883=PLANE('',#13111);
#884=PLANE('',#13112);
#885=PLANE('',#13113);
#886=PLANE('',#13114);
#887=PLANE('',#13115);
#888=PLANE('',#13116);
#889=PLANE('',#13117);
#890=PLANE('',#13118);
#891=PLANE('',#13119);
#892=PLANE('',#13120);
#893=PLANE('',#13121);
#894=PLANE('',#13123);
#895=PLANE('',#13124);
#896=PLANE('',#13125);
#897=PLANE('',#13126);
#898=PLANE('',#13127);
#899=PLANE('',#13134);
#900=PLANE('',#13138);
#901=PLANE('',#13146);
#902=PLANE('',#13147);
#903=PLANE('',#13148);
#904=PLANE('',#13149);
#905=PLANE('',#13150);
#906=PLANE('',#13151);
#907=PLANE('',#13152);
#908=PLANE('',#13156);
#909=PLANE('',#13157);
#910=PLANE('',#13158);
#911=PLANE('',#13159);
#912=PLANE('',#13161);
#913=PLANE('',#13162);
#914=PLANE('',#13163);
#915=PLANE('',#13164);
#916=PLANE('',#13165);
#917=PLANE('',#13172);
#918=PLANE('',#13176);
#919=PLANE('',#13184);
#920=PLANE('',#13185);
#921=PLANE('',#13186);
#922=PLANE('',#13187);
#923=PLANE('',#13188);
#924=PLANE('',#13189);
#925=PLANE('',#13190);
#926=PLANE('',#13194);
#927=PLANE('',#13195);
#928=PLANE('',#13196);
#929=PLANE('',#13197);
#930=PLANE('',#13202);
#931=PLANE('',#13207);
#932=PLANE('',#13216);
#933=PLANE('',#13217);
#934=PLANE('',#13222);
#935=PLANE('',#13225);
#936=PLANE('',#13245);
#937=PLANE('',#13246);
#938=PLANE('',#13247);
#939=PLANE('',#13248);
#940=PLANE('',#13249);
#941=PLANE('',#13250);
#942=PLANE('',#13251);
#943=PLANE('',#13252);
#944=PLANE('',#13272);
#945=PLANE('',#13276);
#946=PLANE('',#13277);
#947=PLANE('',#13297);
#948=PLANE('',#13301);
#949=PLANE('',#13302);
#950=PLANE('',#13307);
#951=PLANE('',#13310);
#952=PLANE('',#13330);
#953=PLANE('',#13331);
#954=PLANE('',#13332);
#955=PLANE('',#13333);
#956=PLANE('',#13334);
#957=PLANE('',#13335);
#958=PLANE('',#13336);
#959=PLANE('',#13337);
#960=PLANE('',#13357);
#961=PLANE('',#13361);
#962=PLANE('',#13362);
#963=PLANE('',#13382);
#964=PLANE('',#13386);
#965=PLANE('',#13387);
#966=PLANE('',#13389);
#967=PLANE('',#13397);
#968=PLANE('',#13405);
#969=PLANE('',#13406);
#970=PLANE('',#13407);
#971=PLANE('',#13408);
#972=PLANE('',#13409);
#973=PLANE('',#13410);
#974=PLANE('',#13411);
#975=PLANE('',#13412);
#976=PLANE('',#13413);
#977=PLANE('',#13429);
#978=PLANE('',#13432);
#979=PLANE('',#13444);
#980=PLANE('',#13453);
#981=PLANE('',#13484);
#982=PLANE('',#13489);
#983=PLANE('',#13494);
#984=PLANE('',#13500);
#985=PLANE('',#13505);
#986=PLANE('',#13514);
#987=PLANE('',#13518);
#988=PLANE('',#13519);
#989=PLANE('',#13521);
#990=PLANE('',#13526);
#991=PLANE('',#13529);
#992=PLANE('',#13534);
#993=PLANE('',#13543);
#994=PLANE('',#13544);
#995=PLANE('',#13545);
#996=PLANE('',#13546);
#997=PLANE('',#13547);
#998=PLANE('',#13548);
#999=PLANE('',#13549);
#1000=PLANE('',#13550);
#1001=PLANE('',#13551);
#1002=PLANE('',#13553);
#1003=PLANE('',#13561);
#1004=PLANE('',#13571);
#1005=PLANE('',#13572);
#1006=PLANE('',#13573);
#1007=PLANE('',#13574);
#1008=PLANE('',#13577);
#1009=PLANE('',#13580);
#1010=PLANE('',#13581);
#1011=PLANE('',#13582);
#1012=PLANE('',#13583);
#1013=PLANE('',#13584);
#1014=PLANE('',#13585);
#1015=PLANE('',#13586);
#1016=PLANE('',#13587);
#1017=PLANE('',#13588);
#1018=PLANE('',#13589);
#1019=PLANE('',#13590);
#1020=PLANE('',#13591);
#1021=PLANE('',#13592);
#1022=PLANE('',#13593);
#1023=PLANE('',#13594);
#1024=PLANE('',#13595);
#1025=PLANE('',#13596);
#1026=PLANE('',#13597);
#1027=PLANE('',#13598);
#1028=PLANE('',#13599);
#1029=PLANE('',#13600);
#1030=PLANE('',#13601);
#1031=PLANE('',#13602);
#1032=PLANE('',#13603);
#1033=PLANE('',#13604);
#1034=PLANE('',#13605);
#1035=PLANE('',#13606);
#1036=PLANE('',#13607);
#1037=PLANE('',#13608);
#1038=PLANE('',#13609);
#1039=PLANE('',#13610);
#1040=PLANE('',#13611);
#1041=PLANE('',#13612);
#1042=PLANE('',#13613);
#1043=PLANE('',#13614);
#1044=PLANE('',#13615);
#1045=PLANE('',#13616);
#1046=PLANE('',#13617);
#1047=PLANE('',#13618);
#1048=PLANE('',#13619);
#1049=PLANE('',#13620);
#1050=PLANE('',#13621);
#1051=PLANE('',#13622);
#1052=PLANE('',#13623);
#1053=PLANE('',#13624);
#1054=PLANE('',#13625);
#1055=PLANE('',#13626);
#1056=PLANE('',#13627);
#1057=PLANE('',#13628);
#1058=PLANE('',#13629);
#1059=PLANE('',#13630);
#1060=PLANE('',#13631);
#1061=PLANE('',#13632);
#1062=PLANE('',#13633);
#1063=PLANE('',#13634);
#1064=PLANE('',#13635);
#1065=PLANE('',#13636);
#1066=PLANE('',#13637);
#1067=PLANE('',#13638);
#1068=PLANE('',#13639);
#1069=PLANE('',#13640);
#1070=PLANE('',#13641);
#1071=PLANE('',#13642);
#1072=PLANE('',#13643);
#1073=PLANE('',#13644);
#1074=PLANE('',#13645);
#1075=PLANE('',#13646);
#1076=PLANE('',#13647);
#1077=PLANE('',#13648);
#1078=PLANE('',#13649);
#1079=PLANE('',#13650);
#1080=PLANE('',#13651);
#1081=PLANE('',#13652);
#1082=PLANE('',#13653);
#1083=PLANE('',#13654);
#1084=PLANE('',#13655);
#1085=PLANE('',#13656);
#1086=PLANE('',#13657);
#1087=PLANE('',#13658);
#1088=PLANE('',#13659);
#1089=PLANE('',#13660);
#1090=PLANE('',#13661);
#1091=PLANE('',#13662);
#1092=PLANE('',#13663);
#1093=PLANE('',#13664);
#1094=PLANE('',#13665);
#1095=PLANE('',#13666);
#1096=PLANE('',#13667);
#1097=PLANE('',#13668);
#1098=PLANE('',#13669);
#1099=PLANE('',#13670);
#1100=PLANE('',#13671);
#1101=PLANE('',#13672);
#1102=PLANE('',#13673);
#1103=PLANE('',#13674);
#1104=PLANE('',#13675);
#1105=PLANE('',#13676);
#1106=PLANE('',#13677);
#1107=PLANE('',#13678);
#1108=PLANE('',#13679);
#1109=PLANE('',#13680);
#1110=PLANE('',#13681);
#1111=PLANE('',#13682);
#1112=PLANE('',#13683);
#1113=PLANE('',#13684);
#1114=PLANE('',#13685);
#1115=PLANE('',#13686);
#1116=PLANE('',#13687);
#1117=PLANE('',#13688);
#1118=PLANE('',#13689);
#1119=PLANE('',#13690);
#1120=PLANE('',#13691);
#1121=PLANE('',#13692);
#1122=PLANE('',#13693);
#1123=PLANE('',#13694);
#1124=PLANE('',#13695);
#1125=PLANE('',#13696);
#1126=PLANE('',#13697);
#1127=PLANE('',#13698);
#1128=PLANE('',#13699);
#1129=PLANE('',#13700);
#1130=PLANE('',#13701);
#1131=PLANE('',#13702);
#1132=PLANE('',#13703);
#1133=PLANE('',#13704);
#1134=PLANE('',#13705);
#1135=PLANE('',#13706);
#1136=PLANE('',#13707);
#1137=PLANE('',#13708);
#1138=PLANE('',#13709);
#1139=PLANE('',#13710);
#1140=PLANE('',#13711);
#1141=PLANE('',#13712);
#1142=PLANE('',#13713);
#1143=PLANE('',#13714);
#1144=PLANE('',#13715);
#1145=PLANE('',#13716);
#1146=PLANE('',#13717);
#1147=PLANE('',#13718);
#1148=PLANE('',#13719);
#1149=PLANE('',#13720);
#1150=PLANE('',#13721);
#1151=PLANE('',#13722);
#1152=PLANE('',#13723);
#1153=PLANE('',#13724);
#1154=PLANE('',#13725);
#1155=PLANE('',#13726);
#1156=PLANE('',#13727);
#1157=PLANE('',#13728);
#1158=PLANE('',#13729);
#1159=PLANE('',#13730);
#1160=PLANE('',#13731);
#1161=PLANE('',#13732);
#1162=PLANE('',#13733);
#1163=PLANE('',#13734);
#1164=PLANE('',#13735);
#1165=PLANE('',#13736);
#1166=PLANE('',#13737);
#1167=PLANE('',#13738);
#1168=PLANE('',#13739);
#1169=PLANE('',#13740);
#1170=PLANE('',#13741);
#1171=PLANE('',#13742);
#1172=PLANE('',#13746);
#1173=PLANE('',#13747);
#1174=PLANE('',#13752);
#1175=PLANE('',#13756);
#1176=PLANE('',#13757);
#1177=PLANE('',#13760);
#1178=PLANE('',#13761);
#1179=PLANE('',#13762);
#1180=PLANE('',#13763);
#1181=PLANE('',#13764);
#1182=PLANE('',#13771);
#1183=PLANE('',#13773);
#1184=PLANE('',#13774);
#1185=PLANE('',#13775);
#1186=PLANE('',#13776);
#1187=PLANE('',#13777);
#1188=PLANE('',#13778);
#1189=PLANE('',#13779);
#1190=PLANE('',#13780);
#1191=PLANE('',#13788);
#1192=PLANE('',#13798);
#1193=PLANE('',#13802);
#1194=PLANE('',#13803);
#1195=PLANE('',#13804);
#1196=PLANE('',#13806);
#1197=PLANE('',#13807);
#1198=PLANE('',#13808);
#1199=PLANE('',#13810);
#1200=PLANE('',#13811);
#1201=PLANE('',#13813);
#1202=PLANE('',#13814);
#1203=PLANE('',#13815);
#1204=PLANE('',#13820);
#1205=PLANE('',#13821);
#1206=PLANE('',#13829);
#1207=PLANE('',#13830);
#1208=PLANE('',#13838);
#1209=PLANE('',#13839);
#1210=PLANE('',#13847);
#1211=PLANE('',#13848);
#1212=PLANE('',#13856);
#1213=PLANE('',#13857);
#1214=PLANE('',#13859);
#1215=PLANE('',#13860);
#1216=PLANE('',#13861);
#1217=PLANE('',#13862);
#1218=PLANE('',#13863);
#1219=PLANE('',#13864);
#1220=PLANE('',#13866);
#1221=PLANE('',#13867);
#1222=PLANE('',#13868);
#1223=PLANE('',#13869);
#1224=PLANE('',#13870);
#1225=PLANE('',#13871);
#1226=PLANE('',#13876);
#1227=PLANE('',#13877);
#1228=PLANE('',#13878);
#1229=PLANE('',#13879);
#1230=PLANE('',#13887);
#1231=PLANE('',#13888);
#1232=PLANE('',#13890);
#1233=PLANE('',#13891);
#1234=PLANE('',#13895);
#1235=PLANE('',#13903);
#1236=PLANE('',#13904);
#1237=PLANE('',#13912);
#1238=PLANE('',#13913);
#1239=PLANE('',#13921);
#1240=PLANE('',#13922);
#1241=PLANE('',#13924);
#1242=PLANE('',#13925);
#1243=PLANE('',#13926);
#1244=PLANE('',#13927);
#1245=PLANE('',#13954);
#1246=PLANE('',#13955);
#1247=PLANE('',#13958);
#1248=PLANE('',#13961);
#1249=PLANE('',#13964);
#1250=PLANE('',#13967);
#1251=PLANE('',#13970);
#1252=PLANE('',#13973);
#1253=PLANE('',#13976);
#1254=PLANE('',#13979);
#1255=PLANE('',#13982);
#1256=PLANE('',#13985);
#1257=PLANE('',#13988);
#1258=PLANE('',#13991);
#1259=PLANE('',#13994);
#1260=PLANE('',#13997);
#1261=PLANE('',#14000);
#1262=PLANE('',#14003);
#1263=PLANE('',#14006);
#1264=PLANE('',#14009);
#1265=PLANE('',#14012);
#1266=PLANE('',#14013);
#1267=PLANE('',#14023);
#1268=PLANE('',#14024);
#1269=PLANE('',#14026);
#1270=PLANE('',#14034);
#1271=PLANE('',#14042);
#1272=PLANE('',#14043);
#1273=PLANE('',#14044);
#1274=PLANE('',#14045);
#1275=PLANE('',#14046);
#1276=PLANE('',#14047);
#1277=PLANE('',#14048);
#1278=PLANE('',#14049);
#1279=PLANE('',#14050);
#1280=PLANE('',#14052);
#1281=PLANE('',#14060);
#1282=PLANE('',#14068);
#1283=PLANE('',#14069);
#1284=PLANE('',#14070);
#1285=PLANE('',#14071);
#1286=PLANE('',#14072);
#1287=PLANE('',#14073);
#1288=PLANE('',#14074);
#1289=PLANE('',#14075);
#1290=PLANE('',#14076);
#1291=PLANE('',#14148);
#1292=PLANE('',#14149);
#1293=FACE_OUTER_BOUND('',#1974,.T.);
#1294=FACE_OUTER_BOUND('',#1975,.T.);
#1295=FACE_OUTER_BOUND('',#1976,.T.);
#1296=FACE_OUTER_BOUND('',#1977,.T.);
#1297=FACE_OUTER_BOUND('',#1978,.T.);
#1298=FACE_OUTER_BOUND('',#1979,.T.);
#1299=FACE_OUTER_BOUND('',#1980,.T.);
#1300=FACE_OUTER_BOUND('',#1981,.T.);
#1301=FACE_OUTER_BOUND('',#1982,.T.);
#1302=FACE_OUTER_BOUND('',#1983,.T.);
#1303=FACE_OUTER_BOUND('',#1984,.T.);
#1304=FACE_OUTER_BOUND('',#1985,.T.);
#1305=FACE_OUTER_BOUND('',#1986,.T.);
#1306=FACE_OUTER_BOUND('',#1987,.T.);
#1307=FACE_OUTER_BOUND('',#1988,.T.);
#1308=FACE_OUTER_BOUND('',#1999,.T.);
#1309=FACE_OUTER_BOUND('',#2010,.T.);
#1310=FACE_OUTER_BOUND('',#2011,.T.);
#1311=FACE_OUTER_BOUND('',#2012,.T.);
#1312=FACE_OUTER_BOUND('',#2013,.T.);
#1313=FACE_OUTER_BOUND('',#2014,.T.);
#1314=FACE_OUTER_BOUND('',#2015,.T.);
#1315=FACE_OUTER_BOUND('',#2016,.T.);
#1316=FACE_OUTER_BOUND('',#2017,.T.);
#1317=FACE_OUTER_BOUND('',#2018,.T.);
#1318=FACE_OUTER_BOUND('',#2019,.T.);
#1319=FACE_OUTER_BOUND('',#2020,.T.);
#1320=FACE_OUTER_BOUND('',#2021,.T.);
#1321=FACE_OUTER_BOUND('',#2022,.T.);
#1322=FACE_OUTER_BOUND('',#2023,.T.);
#1323=FACE_OUTER_BOUND('',#2024,.T.);
#1324=FACE_OUTER_BOUND('',#2025,.T.);
#1325=FACE_OUTER_BOUND('',#2026,.T.);
#1326=FACE_OUTER_BOUND('',#2027,.T.);
#1327=FACE_OUTER_BOUND('',#2028,.T.);
#1328=FACE_OUTER_BOUND('',#2029,.T.);
#1329=FACE_OUTER_BOUND('',#2030,.T.);
#1330=FACE_OUTER_BOUND('',#2031,.T.);
#1331=FACE_OUTER_BOUND('',#2032,.T.);
#1332=FACE_OUTER_BOUND('',#2035,.T.);
#1333=FACE_OUTER_BOUND('',#2036,.T.);
#1334=FACE_OUTER_BOUND('',#2037,.T.);
#1335=FACE_OUTER_BOUND('',#2038,.T.);
#1336=FACE_OUTER_BOUND('',#2039,.T.);
#1337=FACE_OUTER_BOUND('',#2040,.T.);
#1338=FACE_OUTER_BOUND('',#2041,.T.);
#1339=FACE_OUTER_BOUND('',#2042,.T.);
#1340=FACE_OUTER_BOUND('',#2043,.T.);
#1341=FACE_OUTER_BOUND('',#2044,.T.);
#1342=FACE_OUTER_BOUND('',#2045,.T.);
#1343=FACE_OUTER_BOUND('',#2046,.T.);
#1344=FACE_OUTER_BOUND('',#2047,.T.);
#1345=FACE_OUTER_BOUND('',#2050,.T.);
#1346=FACE_OUTER_BOUND('',#2051,.T.);
#1347=FACE_OUTER_BOUND('',#2052,.T.);
#1348=FACE_OUTER_BOUND('',#2053,.T.);
#1349=FACE_OUTER_BOUND('',#2054,.T.);
#1350=FACE_OUTER_BOUND('',#2055,.T.);
#1351=FACE_OUTER_BOUND('',#2056,.T.);
#1352=FACE_OUTER_BOUND('',#2062,.T.);
#1353=FACE_OUTER_BOUND('',#2063,.T.);
#1354=FACE_OUTER_BOUND('',#2064,.T.);
#1355=FACE_OUTER_BOUND('',#2065,.T.);
#1356=FACE_OUTER_BOUND('',#2066,.T.);
#1357=FACE_OUTER_BOUND('',#2067,.T.);
#1358=FACE_OUTER_BOUND('',#2068,.T.);
#1359=FACE_OUTER_BOUND('',#2069,.T.);
#1360=FACE_OUTER_BOUND('',#2072,.T.);
#1361=FACE_OUTER_BOUND('',#2073,.T.);
#1362=FACE_OUTER_BOUND('',#2078,.T.);
#1363=FACE_OUTER_BOUND('',#2079,.T.);
#1364=FACE_OUTER_BOUND('',#2080,.T.);
#1365=FACE_OUTER_BOUND('',#2081,.T.);
#1366=FACE_OUTER_BOUND('',#2082,.T.);
#1367=FACE_OUTER_BOUND('',#2083,.T.);
#1368=FACE_OUTER_BOUND('',#2084,.T.);
#1369=FACE_OUTER_BOUND('',#2085,.T.);
#1370=FACE_OUTER_BOUND('',#2086,.T.);
#1371=FACE_OUTER_BOUND('',#2087,.T.);
#1372=FACE_OUTER_BOUND('',#2088,.T.);
#1373=FACE_OUTER_BOUND('',#2089,.T.);
#1374=FACE_OUTER_BOUND('',#2090,.T.);
#1375=FACE_OUTER_BOUND('',#2091,.T.);
#1376=FACE_OUTER_BOUND('',#2092,.T.);
#1377=FACE_OUTER_BOUND('',#2093,.T.);
#1378=FACE_OUTER_BOUND('',#2094,.T.);
#1379=FACE_OUTER_BOUND('',#2095,.T.);
#1380=FACE_OUTER_BOUND('',#2096,.T.);
#1381=FACE_OUTER_BOUND('',#2099,.T.);
#1382=FACE_OUTER_BOUND('',#2100,.T.);
#1383=FACE_OUTER_BOUND('',#2101,.T.);
#1384=FACE_OUTER_BOUND('',#2102,.T.);
#1385=FACE_OUTER_BOUND('',#2103,.T.);
#1386=FACE_OUTER_BOUND('',#2106,.T.);
#1387=FACE_OUTER_BOUND('',#2107,.T.);
#1388=FACE_OUTER_BOUND('',#2108,.T.);
#1389=FACE_OUTER_BOUND('',#2109,.T.);
#1390=FACE_OUTER_BOUND('',#2110,.T.);
#1391=FACE_OUTER_BOUND('',#2111,.T.);
#1392=FACE_OUTER_BOUND('',#2112,.T.);
#1393=FACE_OUTER_BOUND('',#2113,.T.);
#1394=FACE_OUTER_BOUND('',#2114,.T.);
#1395=FACE_OUTER_BOUND('',#2115,.T.);
#1396=FACE_OUTER_BOUND('',#2116,.T.);
#1397=FACE_OUTER_BOUND('',#2117,.T.);
#1398=FACE_OUTER_BOUND('',#2118,.T.);
#1399=FACE_OUTER_BOUND('',#2119,.T.);
#1400=FACE_OUTER_BOUND('',#2120,.T.);
#1401=FACE_OUTER_BOUND('',#2121,.T.);
#1402=FACE_OUTER_BOUND('',#2122,.T.);
#1403=FACE_OUTER_BOUND('',#2123,.T.);
#1404=FACE_OUTER_BOUND('',#2124,.T.);
#1405=FACE_OUTER_BOUND('',#2127,.T.);
#1406=FACE_OUTER_BOUND('',#2128,.T.);
#1407=FACE_OUTER_BOUND('',#2129,.T.);
#1408=FACE_OUTER_BOUND('',#2130,.T.);
#1409=FACE_OUTER_BOUND('',#2131,.T.);
#1410=FACE_OUTER_BOUND('',#2134,.T.);
#1411=FACE_OUTER_BOUND('',#2135,.T.);
#1412=FACE_OUTER_BOUND('',#2137,.T.);
#1413=FACE_OUTER_BOUND('',#2138,.T.);
#1414=FACE_OUTER_BOUND('',#2140,.T.);
#1415=FACE_OUTER_BOUND('',#2141,.T.);
#1416=FACE_OUTER_BOUND('',#2142,.T.);
#1417=FACE_OUTER_BOUND('',#2143,.T.);
#1418=FACE_OUTER_BOUND('',#2146,.T.);
#1419=FACE_OUTER_BOUND('',#2149,.T.);
#1420=FACE_OUTER_BOUND('',#2150,.T.);
#1421=FACE_OUTER_BOUND('',#2153,.T.);
#1422=FACE_OUTER_BOUND('',#2154,.T.);
#1423=FACE_OUTER_BOUND('',#2155,.T.);
#1424=FACE_OUTER_BOUND('',#2156,.T.);
#1425=FACE_OUTER_BOUND('',#2157,.T.);
#1426=FACE_OUTER_BOUND('',#2158,.T.);
#1427=FACE_OUTER_BOUND('',#2159,.T.);
#1428=FACE_OUTER_BOUND('',#2160,.T.);
#1429=FACE_OUTER_BOUND('',#2161,.T.);
#1430=FACE_OUTER_BOUND('',#2163,.T.);
#1431=FACE_OUTER_BOUND('',#2165,.T.);
#1432=FACE_OUTER_BOUND('',#2166,.T.);
#1433=FACE_OUTER_BOUND('',#2172,.T.);
#1434=FACE_OUTER_BOUND('',#2173,.T.);
#1435=FACE_OUTER_BOUND('',#2179,.T.);
#1436=FACE_OUTER_BOUND('',#2180,.T.);
#1437=FACE_OUTER_BOUND('',#2181,.T.);
#1438=FACE_OUTER_BOUND('',#2182,.T.);
#1439=FACE_OUTER_BOUND('',#2183,.T.);
#1440=FACE_OUTER_BOUND('',#2184,.T.);
#1441=FACE_OUTER_BOUND('',#2185,.T.);
#1442=FACE_OUTER_BOUND('',#2186,.T.);
#1443=FACE_OUTER_BOUND('',#2187,.T.);
#1444=FACE_OUTER_BOUND('',#2189,.T.);
#1445=FACE_OUTER_BOUND('',#2190,.T.);
#1446=FACE_OUTER_BOUND('',#2196,.T.);
#1447=FACE_OUTER_BOUND('',#2202,.T.);
#1448=FACE_OUTER_BOUND('',#2203,.T.);
#1449=FACE_OUTER_BOUND('',#2204,.T.);
#1450=FACE_OUTER_BOUND('',#2205,.T.);
#1451=FACE_OUTER_BOUND('',#2206,.T.);
#1452=FACE_OUTER_BOUND('',#2207,.T.);
#1453=FACE_OUTER_BOUND('',#2208,.T.);
#1454=FACE_OUTER_BOUND('',#2210,.T.);
#1455=FACE_OUTER_BOUND('',#2211,.T.);
#1456=FACE_OUTER_BOUND('',#2217,.T.);
#1457=FACE_OUTER_BOUND('',#2223,.T.);
#1458=FACE_OUTER_BOUND('',#2224,.T.);
#1459=FACE_OUTER_BOUND('',#2227,.T.);
#1460=FACE_OUTER_BOUND('',#2233,.T.);
#1461=FACE_OUTER_BOUND('',#2234,.T.);
#1462=FACE_OUTER_BOUND('',#2235,.T.);
#1463=FACE_OUTER_BOUND('',#2236,.T.);
#1464=FACE_OUTER_BOUND('',#2237,.T.);
#1465=FACE_OUTER_BOUND('',#2238,.T.);
#1466=FACE_OUTER_BOUND('',#2239,.T.);
#1467=FACE_OUTER_BOUND('',#2240,.T.);
#1468=FACE_OUTER_BOUND('',#2242,.T.);
#1469=FACE_OUTER_BOUND('',#2244,.T.);
#1470=FACE_OUTER_BOUND('',#2245,.T.);
#1471=FACE_OUTER_BOUND('',#2246,.T.);
#1472=FACE_OUTER_BOUND('',#2247,.T.);
#1473=FACE_OUTER_BOUND('',#2253,.T.);
#1474=FACE_OUTER_BOUND('',#2254,.T.);
#1475=FACE_OUTER_BOUND('',#2255,.T.);
#1476=FACE_OUTER_BOUND('',#2256,.T.);
#1477=FACE_OUTER_BOUND('',#2257,.T.);
#1478=FACE_OUTER_BOUND('',#2258,.T.);
#1479=FACE_OUTER_BOUND('',#2259,.T.);
#1480=FACE_OUTER_BOUND('',#2260,.T.);
#1481=FACE_OUTER_BOUND('',#2261,.T.);
#1482=FACE_OUTER_BOUND('',#2263,.T.);
#1483=FACE_OUTER_BOUND('',#2264,.T.);
#1484=FACE_OUTER_BOUND('',#2270,.T.);
#1485=FACE_OUTER_BOUND('',#2276,.T.);
#1486=FACE_OUTER_BOUND('',#2277,.T.);
#1487=FACE_OUTER_BOUND('',#2278,.T.);
#1488=FACE_OUTER_BOUND('',#2279,.T.);
#1489=FACE_OUTER_BOUND('',#2280,.T.);
#1490=FACE_OUTER_BOUND('',#2281,.T.);
#1491=FACE_OUTER_BOUND('',#2282,.T.);
#1492=FACE_OUTER_BOUND('',#2284,.T.);
#1493=FACE_OUTER_BOUND('',#2285,.T.);
#1494=FACE_OUTER_BOUND('',#2291,.T.);
#1495=FACE_OUTER_BOUND('',#2297,.T.);
#1496=FACE_OUTER_BOUND('',#2298,.T.);
#1497=FACE_OUTER_BOUND('',#2299,.T.);
#1498=FACE_OUTER_BOUND('',#2300,.T.);
#1499=FACE_OUTER_BOUND('',#2301,.T.);
#1500=FACE_OUTER_BOUND('',#2303,.T.);
#1501=FACE_OUTER_BOUND('',#2304,.T.);
#1502=FACE_OUTER_BOUND('',#2305,.T.);
#1503=FACE_OUTER_BOUND('',#2306,.T.);
#1504=FACE_OUTER_BOUND('',#2307,.T.);
#1505=FACE_OUTER_BOUND('',#2308,.T.);
#1506=FACE_OUTER_BOUND('',#2309,.T.);
#1507=FACE_OUTER_BOUND('',#2310,.T.);
#1508=FACE_OUTER_BOUND('',#2311,.T.);
#1509=FACE_OUTER_BOUND('',#2312,.T.);
#1510=FACE_OUTER_BOUND('',#2313,.T.);
#1511=FACE_OUTER_BOUND('',#2314,.T.);
#1512=FACE_OUTER_BOUND('',#2315,.T.);
#1513=FACE_OUTER_BOUND('',#2316,.T.);
#1514=FACE_OUTER_BOUND('',#2317,.T.);
#1515=FACE_OUTER_BOUND('',#2318,.T.);
#1516=FACE_OUTER_BOUND('',#2319,.T.);
#1517=FACE_OUTER_BOUND('',#2321,.T.);
#1518=FACE_OUTER_BOUND('',#2322,.T.);
#1519=FACE_OUTER_BOUND('',#2324,.T.);
#1520=FACE_OUTER_BOUND('',#2325,.T.);
#1521=FACE_OUTER_BOUND('',#2326,.T.);
#1522=FACE_OUTER_BOUND('',#2327,.T.);
#1523=FACE_OUTER_BOUND('',#2329,.T.);
#1524=FACE_OUTER_BOUND('',#2330,.T.);
#1525=FACE_OUTER_BOUND('',#2331,.T.);
#1526=FACE_OUTER_BOUND('',#2332,.T.);
#1527=FACE_OUTER_BOUND('',#2334,.T.);
#1528=FACE_OUTER_BOUND('',#2335,.T.);
#1529=FACE_OUTER_BOUND('',#2336,.T.);
#1530=FACE_OUTER_BOUND('',#2337,.T.);
#1531=FACE_OUTER_BOUND('',#2338,.T.);
#1532=FACE_OUTER_BOUND('',#2339,.T.);
#1533=FACE_OUTER_BOUND('',#2340,.T.);
#1534=FACE_OUTER_BOUND('',#2341,.T.);
#1535=FACE_OUTER_BOUND('',#2342,.T.);
#1536=FACE_OUTER_BOUND('',#2343,.T.);
#1537=FACE_OUTER_BOUND('',#2344,.T.);
#1538=FACE_OUTER_BOUND('',#2345,.T.);
#1539=FACE_OUTER_BOUND('',#2346,.T.);
#1540=FACE_OUTER_BOUND('',#2347,.T.);
#1541=FACE_OUTER_BOUND('',#2348,.T.);
#1542=FACE_OUTER_BOUND('',#2349,.T.);
#1543=FACE_OUTER_BOUND('',#2350,.T.);
#1544=FACE_OUTER_BOUND('',#2351,.T.);
#1545=FACE_OUTER_BOUND('',#2352,.T.);
#1546=FACE_OUTER_BOUND('',#2353,.T.);
#1547=FACE_OUTER_BOUND('',#2354,.T.);
#1548=FACE_OUTER_BOUND('',#2355,.T.);
#1549=FACE_OUTER_BOUND('',#2356,.T.);
#1550=FACE_OUTER_BOUND('',#2357,.T.);
#1551=FACE_OUTER_BOUND('',#2359,.T.);
#1552=FACE_OUTER_BOUND('',#2360,.T.);
#1553=FACE_OUTER_BOUND('',#2362,.T.);
#1554=FACE_OUTER_BOUND('',#2363,.T.);
#1555=FACE_OUTER_BOUND('',#2365,.T.);
#1556=FACE_OUTER_BOUND('',#2366,.T.);
#1557=FACE_OUTER_BOUND('',#2368,.T.);
#1558=FACE_OUTER_BOUND('',#2369,.T.);
#1559=FACE_OUTER_BOUND('',#2371,.T.);
#1560=FACE_OUTER_BOUND('',#2372,.T.);
#1561=FACE_OUTER_BOUND('',#2373,.T.);
#1562=FACE_OUTER_BOUND('',#2374,.T.);
#1563=FACE_OUTER_BOUND('',#2375,.T.);
#1564=FACE_OUTER_BOUND('',#2376,.T.);
#1565=FACE_OUTER_BOUND('',#2377,.T.);
#1566=FACE_OUTER_BOUND('',#2378,.T.);
#1567=FACE_OUTER_BOUND('',#2379,.T.);
#1568=FACE_OUTER_BOUND('',#2380,.T.);
#1569=FACE_OUTER_BOUND('',#2381,.T.);
#1570=FACE_OUTER_BOUND('',#2382,.T.);
#1571=FACE_OUTER_BOUND('',#2383,.T.);
#1572=FACE_OUTER_BOUND('',#2384,.T.);
#1573=FACE_OUTER_BOUND('',#2385,.T.);
#1574=FACE_OUTER_BOUND('',#2387,.T.);
#1575=FACE_OUTER_BOUND('',#2388,.T.);
#1576=FACE_OUTER_BOUND('',#2389,.T.);
#1577=FACE_OUTER_BOUND('',#2390,.T.);
#1578=FACE_OUTER_BOUND('',#2391,.T.);
#1579=FACE_OUTER_BOUND('',#2392,.T.);
#1580=FACE_OUTER_BOUND('',#2393,.T.);
#1581=FACE_OUTER_BOUND('',#2394,.T.);
#1582=FACE_OUTER_BOUND('',#2395,.T.);
#1583=FACE_OUTER_BOUND('',#2396,.T.);
#1584=FACE_OUTER_BOUND('',#2397,.T.);
#1585=FACE_OUTER_BOUND('',#2398,.T.);
#1586=FACE_OUTER_BOUND('',#2399,.T.);
#1587=FACE_OUTER_BOUND('',#2400,.T.);
#1588=FACE_OUTER_BOUND('',#2401,.T.);
#1589=FACE_OUTER_BOUND('',#2402,.T.);
#1590=FACE_OUTER_BOUND('',#2403,.T.);
#1591=FACE_OUTER_BOUND('',#2404,.T.);
#1592=FACE_OUTER_BOUND('',#2405,.T.);
#1593=FACE_OUTER_BOUND('',#2406,.T.);
#1594=FACE_OUTER_BOUND('',#2407,.T.);
#1595=FACE_OUTER_BOUND('',#2408,.T.);
#1596=FACE_OUTER_BOUND('',#2409,.T.);
#1597=FACE_OUTER_BOUND('',#2410,.T.);
#1598=FACE_OUTER_BOUND('',#2411,.T.);
#1599=FACE_OUTER_BOUND('',#2412,.T.);
#1600=FACE_OUTER_BOUND('',#2413,.T.);
#1601=FACE_OUTER_BOUND('',#2414,.T.);
#1602=FACE_OUTER_BOUND('',#2415,.T.);
#1603=FACE_OUTER_BOUND('',#2416,.T.);
#1604=FACE_OUTER_BOUND('',#2417,.T.);
#1605=FACE_OUTER_BOUND('',#2418,.T.);
#1606=FACE_OUTER_BOUND('',#2419,.T.);
#1607=FACE_OUTER_BOUND('',#2420,.T.);
#1608=FACE_OUTER_BOUND('',#2421,.T.);
#1609=FACE_OUTER_BOUND('',#2422,.T.);
#1610=FACE_OUTER_BOUND('',#2423,.T.);
#1611=FACE_OUTER_BOUND('',#2424,.T.);
#1612=FACE_OUTER_BOUND('',#2425,.T.);
#1613=FACE_OUTER_BOUND('',#2426,.T.);
#1614=FACE_OUTER_BOUND('',#2427,.T.);
#1615=FACE_OUTER_BOUND('',#2428,.T.);
#1616=FACE_OUTER_BOUND('',#2429,.T.);
#1617=FACE_OUTER_BOUND('',#2430,.T.);
#1618=FACE_OUTER_BOUND('',#2431,.T.);
#1619=FACE_OUTER_BOUND('',#2432,.T.);
#1620=FACE_OUTER_BOUND('',#2433,.T.);
#1621=FACE_OUTER_BOUND('',#2434,.T.);
#1622=FACE_OUTER_BOUND('',#2435,.T.);
#1623=FACE_OUTER_BOUND('',#2436,.T.);
#1624=FACE_OUTER_BOUND('',#2437,.T.);
#1625=FACE_OUTER_BOUND('',#2438,.T.);
#1626=FACE_OUTER_BOUND('',#2439,.T.);
#1627=FACE_OUTER_BOUND('',#2440,.T.);
#1628=FACE_OUTER_BOUND('',#2441,.T.);
#1629=FACE_OUTER_BOUND('',#2442,.T.);
#1630=FACE_OUTER_BOUND('',#2443,.T.);
#1631=FACE_OUTER_BOUND('',#2444,.T.);
#1632=FACE_OUTER_BOUND('',#2445,.T.);
#1633=FACE_OUTER_BOUND('',#2446,.T.);
#1634=FACE_OUTER_BOUND('',#2447,.T.);
#1635=FACE_OUTER_BOUND('',#2448,.T.);
#1636=FACE_OUTER_BOUND('',#2449,.T.);
#1637=FACE_OUTER_BOUND('',#2450,.T.);
#1638=FACE_OUTER_BOUND('',#2451,.T.);
#1639=FACE_OUTER_BOUND('',#2452,.T.);
#1640=FACE_OUTER_BOUND('',#2453,.T.);
#1641=FACE_OUTER_BOUND('',#2454,.T.);
#1642=FACE_OUTER_BOUND('',#2455,.T.);
#1643=FACE_OUTER_BOUND('',#2456,.T.);
#1644=FACE_OUTER_BOUND('',#2457,.T.);
#1645=FACE_OUTER_BOUND('',#2458,.T.);
#1646=FACE_OUTER_BOUND('',#2459,.T.);
#1647=FACE_OUTER_BOUND('',#2460,.T.);
#1648=FACE_OUTER_BOUND('',#2461,.T.);
#1649=FACE_OUTER_BOUND('',#2462,.T.);
#1650=FACE_OUTER_BOUND('',#2463,.T.);
#1651=FACE_OUTER_BOUND('',#2464,.T.);
#1652=FACE_OUTER_BOUND('',#2465,.T.);
#1653=FACE_OUTER_BOUND('',#2466,.T.);
#1654=FACE_OUTER_BOUND('',#2467,.T.);
#1655=FACE_OUTER_BOUND('',#2468,.T.);
#1656=FACE_OUTER_BOUND('',#2469,.T.);
#1657=FACE_OUTER_BOUND('',#2470,.T.);
#1658=FACE_OUTER_BOUND('',#2471,.T.);
#1659=FACE_OUTER_BOUND('',#2472,.T.);
#1660=FACE_OUTER_BOUND('',#2473,.T.);
#1661=FACE_OUTER_BOUND('',#2474,.T.);
#1662=FACE_OUTER_BOUND('',#2475,.T.);
#1663=FACE_OUTER_BOUND('',#2476,.T.);
#1664=FACE_OUTER_BOUND('',#2477,.T.);
#1665=FACE_OUTER_BOUND('',#2478,.T.);
#1666=FACE_OUTER_BOUND('',#2479,.T.);
#1667=FACE_OUTER_BOUND('',#2480,.T.);
#1668=FACE_OUTER_BOUND('',#2481,.T.);
#1669=FACE_OUTER_BOUND('',#2482,.T.);
#1670=FACE_OUTER_BOUND('',#2483,.T.);
#1671=FACE_OUTER_BOUND('',#2484,.T.);
#1672=FACE_OUTER_BOUND('',#2485,.T.);
#1673=FACE_OUTER_BOUND('',#2486,.T.);
#1674=FACE_OUTER_BOUND('',#2487,.T.);
#1675=FACE_OUTER_BOUND('',#2488,.T.);
#1676=FACE_OUTER_BOUND('',#2489,.T.);
#1677=FACE_OUTER_BOUND('',#2490,.T.);
#1678=FACE_OUTER_BOUND('',#2491,.T.);
#1679=FACE_OUTER_BOUND('',#2492,.T.);
#1680=FACE_OUTER_BOUND('',#2493,.T.);
#1681=FACE_OUTER_BOUND('',#2494,.T.);
#1682=FACE_OUTER_BOUND('',#2495,.T.);
#1683=FACE_OUTER_BOUND('',#2496,.T.);
#1684=FACE_OUTER_BOUND('',#2497,.T.);
#1685=FACE_OUTER_BOUND('',#2498,.T.);
#1686=FACE_OUTER_BOUND('',#2499,.T.);
#1687=FACE_OUTER_BOUND('',#2500,.T.);
#1688=FACE_OUTER_BOUND('',#2501,.T.);
#1689=FACE_OUTER_BOUND('',#2502,.T.);
#1690=FACE_OUTER_BOUND('',#2503,.T.);
#1691=FACE_OUTER_BOUND('',#2504,.T.);
#1692=FACE_OUTER_BOUND('',#2505,.T.);
#1693=FACE_OUTER_BOUND('',#2506,.T.);
#1694=FACE_OUTER_BOUND('',#2507,.T.);
#1695=FACE_OUTER_BOUND('',#2508,.T.);
#1696=FACE_OUTER_BOUND('',#2509,.T.);
#1697=FACE_OUTER_BOUND('',#2510,.T.);
#1698=FACE_OUTER_BOUND('',#2511,.T.);
#1699=FACE_OUTER_BOUND('',#2512,.T.);
#1700=FACE_OUTER_BOUND('',#2513,.T.);
#1701=FACE_OUTER_BOUND('',#2514,.T.);
#1702=FACE_OUTER_BOUND('',#2515,.T.);
#1703=FACE_OUTER_BOUND('',#2516,.T.);
#1704=FACE_OUTER_BOUND('',#2517,.T.);
#1705=FACE_OUTER_BOUND('',#2518,.T.);
#1706=FACE_OUTER_BOUND('',#2519,.T.);
#1707=FACE_OUTER_BOUND('',#2520,.T.);
#1708=FACE_OUTER_BOUND('',#2521,.T.);
#1709=FACE_OUTER_BOUND('',#2522,.T.);
#1710=FACE_OUTER_BOUND('',#2523,.T.);
#1711=FACE_OUTER_BOUND('',#2524,.T.);
#1712=FACE_OUTER_BOUND('',#2525,.T.);
#1713=FACE_OUTER_BOUND('',#2526,.T.);
#1714=FACE_OUTER_BOUND('',#2527,.T.);
#1715=FACE_OUTER_BOUND('',#2528,.T.);
#1716=FACE_OUTER_BOUND('',#2529,.T.);
#1717=FACE_OUTER_BOUND('',#2530,.T.);
#1718=FACE_OUTER_BOUND('',#2531,.T.);
#1719=FACE_OUTER_BOUND('',#2532,.T.);
#1720=FACE_OUTER_BOUND('',#2533,.T.);
#1721=FACE_OUTER_BOUND('',#2534,.T.);
#1722=FACE_OUTER_BOUND('',#2535,.T.);
#1723=FACE_OUTER_BOUND('',#2536,.T.);
#1724=FACE_OUTER_BOUND('',#2537,.T.);
#1725=FACE_OUTER_BOUND('',#2538,.T.);
#1726=FACE_OUTER_BOUND('',#2539,.T.);
#1727=FACE_OUTER_BOUND('',#2540,.T.);
#1728=FACE_OUTER_BOUND('',#2541,.T.);
#1729=FACE_OUTER_BOUND('',#2542,.T.);
#1730=FACE_OUTER_BOUND('',#2543,.T.);
#1731=FACE_OUTER_BOUND('',#2544,.T.);
#1732=FACE_OUTER_BOUND('',#2545,.T.);
#1733=FACE_OUTER_BOUND('',#2546,.T.);
#1734=FACE_OUTER_BOUND('',#2547,.T.);
#1735=FACE_OUTER_BOUND('',#2548,.T.);
#1736=FACE_OUTER_BOUND('',#2549,.T.);
#1737=FACE_OUTER_BOUND('',#2550,.T.);
#1738=FACE_OUTER_BOUND('',#2551,.T.);
#1739=FACE_OUTER_BOUND('',#2552,.T.);
#1740=FACE_OUTER_BOUND('',#2553,.T.);
#1741=FACE_OUTER_BOUND('',#2554,.T.);
#1742=FACE_OUTER_BOUND('',#2555,.T.);
#1743=FACE_OUTER_BOUND('',#2556,.T.);
#1744=FACE_OUTER_BOUND('',#2557,.T.);
#1745=FACE_OUTER_BOUND('',#2558,.T.);
#1746=FACE_OUTER_BOUND('',#2559,.T.);
#1747=FACE_OUTER_BOUND('',#2560,.T.);
#1748=FACE_OUTER_BOUND('',#2562,.T.);
#1749=FACE_OUTER_BOUND('',#2563,.T.);
#1750=FACE_OUTER_BOUND('',#2564,.T.);
#1751=FACE_OUTER_BOUND('',#2565,.T.);
#1752=FACE_OUTER_BOUND('',#2567,.T.);
#1753=FACE_OUTER_BOUND('',#2568,.T.);
#1754=FACE_OUTER_BOUND('',#2569,.T.);
#1755=FACE_OUTER_BOUND('',#2570,.T.);
#1756=FACE_OUTER_BOUND('',#2571,.T.);
#1757=FACE_OUTER_BOUND('',#2572,.T.);
#1758=FACE_OUTER_BOUND('',#2573,.T.);
#1759=FACE_OUTER_BOUND('',#2574,.T.);
#1760=FACE_OUTER_BOUND('',#2576,.T.);
#1761=FACE_OUTER_BOUND('',#2578,.T.);
#1762=FACE_OUTER_BOUND('',#2579,.T.);
#1763=FACE_OUTER_BOUND('',#2580,.T.);
#1764=FACE_OUTER_BOUND('',#2581,.T.);
#1765=FACE_OUTER_BOUND('',#2582,.T.);
#1766=FACE_OUTER_BOUND('',#2583,.T.);
#1767=FACE_OUTER_BOUND('',#2584,.T.);
#1768=FACE_OUTER_BOUND('',#2585,.T.);
#1769=FACE_OUTER_BOUND('',#2586,.T.);
#1770=FACE_OUTER_BOUND('',#2588,.T.);
#1771=FACE_OUTER_BOUND('',#2589,.T.);
#1772=FACE_OUTER_BOUND('',#2590,.T.);
#1773=FACE_OUTER_BOUND('',#2591,.T.);
#1774=FACE_OUTER_BOUND('',#2592,.T.);
#1775=FACE_OUTER_BOUND('',#2593,.T.);
#1776=FACE_OUTER_BOUND('',#2594,.T.);
#1777=FACE_OUTER_BOUND('',#2595,.T.);
#1778=FACE_OUTER_BOUND('',#2596,.T.);
#1779=FACE_OUTER_BOUND('',#2597,.T.);
#1780=FACE_OUTER_BOUND('',#2598,.T.);
#1781=FACE_OUTER_BOUND('',#2599,.T.);
#1782=FACE_OUTER_BOUND('',#2600,.T.);
#1783=FACE_OUTER_BOUND('',#2601,.T.);
#1784=FACE_OUTER_BOUND('',#2602,.T.);
#1785=FACE_OUTER_BOUND('',#2603,.T.);
#1786=FACE_OUTER_BOUND('',#2604,.T.);
#1787=FACE_OUTER_BOUND('',#2605,.T.);
#1788=FACE_OUTER_BOUND('',#2606,.T.);
#1789=FACE_OUTER_BOUND('',#2609,.T.);
#1790=FACE_OUTER_BOUND('',#2611,.T.);
#1791=FACE_OUTER_BOUND('',#2613,.T.);
#1792=FACE_OUTER_BOUND('',#2614,.T.);
#1793=FACE_OUTER_BOUND('',#2615,.T.);
#1794=FACE_OUTER_BOUND('',#2617,.T.);
#1795=FACE_OUTER_BOUND('',#2619,.T.);
#1796=FACE_OUTER_BOUND('',#2620,.T.);
#1797=FACE_OUTER_BOUND('',#2621,.T.);
#1798=FACE_OUTER_BOUND('',#2623,.T.);
#1799=FACE_OUTER_BOUND('',#2625,.T.);
#1800=FACE_OUTER_BOUND('',#2626,.T.);
#1801=FACE_OUTER_BOUND('',#2627,.T.);
#1802=FACE_OUTER_BOUND('',#2629,.T.);
#1803=FACE_OUTER_BOUND('',#2631,.T.);
#1804=FACE_OUTER_BOUND('',#2632,.T.);
#1805=FACE_OUTER_BOUND('',#2633,.T.);
#1806=FACE_OUTER_BOUND('',#2635,.T.);
#1807=FACE_OUTER_BOUND('',#2637,.T.);
#1808=FACE_OUTER_BOUND('',#2638,.T.);
#1809=FACE_OUTER_BOUND('',#2639,.T.);
#1810=FACE_OUTER_BOUND('',#2640,.T.);
#1811=FACE_OUTER_BOUND('',#2641,.T.);
#1812=FACE_OUTER_BOUND('',#2642,.T.);
#1813=FACE_OUTER_BOUND('',#2643,.T.);
#1814=FACE_OUTER_BOUND('',#2644,.T.);
#1815=FACE_OUTER_BOUND('',#2645,.T.);
#1816=FACE_OUTER_BOUND('',#2646,.T.);
#1817=FACE_OUTER_BOUND('',#2647,.T.);
#1818=FACE_OUTER_BOUND('',#2648,.T.);
#1819=FACE_OUTER_BOUND('',#2649,.T.);
#1820=FACE_OUTER_BOUND('',#2650,.T.);
#1821=FACE_OUTER_BOUND('',#2651,.T.);
#1822=FACE_OUTER_BOUND('',#2652,.T.);
#1823=FACE_OUTER_BOUND('',#2653,.T.);
#1824=FACE_OUTER_BOUND('',#2655,.T.);
#1825=FACE_OUTER_BOUND('',#2656,.T.);
#1826=FACE_OUTER_BOUND('',#2657,.T.);
#1827=FACE_OUTER_BOUND('',#2658,.T.);
#1828=FACE_OUTER_BOUND('',#2660,.T.);
#1829=FACE_OUTER_BOUND('',#2661,.T.);
#1830=FACE_OUTER_BOUND('',#2663,.T.);
#1831=FACE_OUTER_BOUND('',#2665,.T.);
#1832=FACE_OUTER_BOUND('',#2667,.T.);
#1833=FACE_OUTER_BOUND('',#2668,.T.);
#1834=FACE_OUTER_BOUND('',#2669,.T.);
#1835=FACE_OUTER_BOUND('',#2671,.T.);
#1836=FACE_OUTER_BOUND('',#2673,.T.);
#1837=FACE_OUTER_BOUND('',#2674,.T.);
#1838=FACE_OUTER_BOUND('',#2675,.T.);
#1839=FACE_OUTER_BOUND('',#2677,.T.);
#1840=FACE_OUTER_BOUND('',#2679,.T.);
#1841=FACE_OUTER_BOUND('',#2680,.T.);
#1842=FACE_OUTER_BOUND('',#2681,.T.);
#1843=FACE_OUTER_BOUND('',#2683,.T.);
#1844=FACE_OUTER_BOUND('',#2685,.T.);
#1845=FACE_OUTER_BOUND('',#2686,.T.);
#1846=FACE_OUTER_BOUND('',#2687,.T.);
#1847=FACE_OUTER_BOUND('',#2688,.T.);
#1848=FACE_OUTER_BOUND('',#2690,.T.);
#1849=FACE_OUTER_BOUND('',#2691,.T.);
#1850=FACE_OUTER_BOUND('',#2692,.T.);
#1851=FACE_OUTER_BOUND('',#2694,.T.);
#1852=FACE_OUTER_BOUND('',#2695,.T.);
#1853=FACE_OUTER_BOUND('',#2696,.T.);
#1854=FACE_OUTER_BOUND('',#2697,.T.);
#1855=FACE_OUTER_BOUND('',#2698,.T.);
#1856=FACE_OUTER_BOUND('',#2699,.T.);
#1857=FACE_OUTER_BOUND('',#2700,.T.);
#1858=FACE_OUTER_BOUND('',#2701,.T.);
#1859=FACE_OUTER_BOUND('',#2702,.T.);
#1860=FACE_OUTER_BOUND('',#2703,.T.);
#1861=FACE_OUTER_BOUND('',#2704,.T.);
#1862=FACE_OUTER_BOUND('',#2705,.T.);
#1863=FACE_OUTER_BOUND('',#2706,.T.);
#1864=FACE_OUTER_BOUND('',#2707,.T.);
#1865=FACE_OUTER_BOUND('',#2708,.T.);
#1866=FACE_OUTER_BOUND('',#2709,.T.);
#1867=FACE_OUTER_BOUND('',#2710,.T.);
#1868=FACE_OUTER_BOUND('',#2711,.T.);
#1869=FACE_OUTER_BOUND('',#2712,.T.);
#1870=FACE_OUTER_BOUND('',#2713,.T.);
#1871=FACE_OUTER_BOUND('',#2714,.T.);
#1872=FACE_OUTER_BOUND('',#2715,.T.);
#1873=FACE_OUTER_BOUND('',#2716,.T.);
#1874=FACE_OUTER_BOUND('',#2717,.T.);
#1875=FACE_OUTER_BOUND('',#2718,.T.);
#1876=FACE_OUTER_BOUND('',#2719,.T.);
#1877=FACE_OUTER_BOUND('',#2720,.T.);
#1878=FACE_OUTER_BOUND('',#2721,.T.);
#1879=FACE_OUTER_BOUND('',#2722,.T.);
#1880=FACE_OUTER_BOUND('',#2723,.T.);
#1881=FACE_OUTER_BOUND('',#2724,.T.);
#1882=FACE_OUTER_BOUND('',#2725,.T.);
#1883=FACE_OUTER_BOUND('',#2726,.T.);
#1884=FACE_OUTER_BOUND('',#2727,.T.);
#1885=FACE_OUTER_BOUND('',#2728,.T.);
#1886=FACE_OUTER_BOUND('',#2729,.T.);
#1887=FACE_OUTER_BOUND('',#2730,.T.);
#1888=FACE_OUTER_BOUND('',#2731,.T.);
#1889=FACE_OUTER_BOUND('',#2732,.T.);
#1890=FACE_OUTER_BOUND('',#2733,.T.);
#1891=FACE_OUTER_BOUND('',#2734,.T.);
#1892=FACE_OUTER_BOUND('',#2735,.T.);
#1893=FACE_OUTER_BOUND('',#2736,.T.);
#1894=FACE_OUTER_BOUND('',#2737,.T.);
#1895=FACE_OUTER_BOUND('',#2738,.T.);
#1896=FACE_OUTER_BOUND('',#2739,.T.);
#1897=FACE_OUTER_BOUND('',#2740,.T.);
#1898=FACE_OUTER_BOUND('',#2741,.T.);
#1899=FACE_OUTER_BOUND('',#2742,.T.);
#1900=FACE_OUTER_BOUND('',#2743,.T.);
#1901=FACE_OUTER_BOUND('',#2744,.T.);
#1902=FACE_OUTER_BOUND('',#2745,.T.);
#1903=FACE_OUTER_BOUND('',#2746,.T.);
#1904=FACE_OUTER_BOUND('',#2747,.T.);
#1905=FACE_OUTER_BOUND('',#2748,.T.);
#1906=FACE_OUTER_BOUND('',#2749,.T.);
#1907=FACE_OUTER_BOUND('',#2750,.T.);
#1908=FACE_OUTER_BOUND('',#2751,.T.);
#1909=FACE_OUTER_BOUND('',#2752,.T.);
#1910=FACE_OUTER_BOUND('',#2753,.T.);
#1911=FACE_OUTER_BOUND('',#2754,.T.);
#1912=FACE_OUTER_BOUND('',#2755,.T.);
#1913=FACE_OUTER_BOUND('',#2756,.T.);
#1914=FACE_OUTER_BOUND('',#2757,.T.);
#1915=FACE_OUTER_BOUND('',#2758,.T.);
#1916=FACE_OUTER_BOUND('',#2759,.T.);
#1917=FACE_OUTER_BOUND('',#2760,.T.);
#1918=FACE_OUTER_BOUND('',#2761,.T.);
#1919=FACE_OUTER_BOUND('',#2762,.T.);
#1920=FACE_OUTER_BOUND('',#2763,.T.);
#1921=FACE_OUTER_BOUND('',#2764,.T.);
#1922=FACE_OUTER_BOUND('',#2765,.T.);
#1923=FACE_OUTER_BOUND('',#2766,.T.);
#1924=FACE_OUTER_BOUND('',#2767,.T.);
#1925=FACE_OUTER_BOUND('',#2768,.T.);
#1926=FACE_OUTER_BOUND('',#2769,.T.);
#1927=FACE_OUTER_BOUND('',#2770,.T.);
#1928=FACE_OUTER_BOUND('',#2771,.T.);
#1929=FACE_OUTER_BOUND('',#2772,.T.);
#1930=FACE_OUTER_BOUND('',#2773,.T.);
#1931=FACE_OUTER_BOUND('',#2775,.T.);
#1932=FACE_OUTER_BOUND('',#2776,.T.);
#1933=FACE_OUTER_BOUND('',#2777,.T.);
#1934=FACE_OUTER_BOUND('',#2778,.T.);
#1935=FACE_OUTER_BOUND('',#2780,.T.);
#1936=FACE_OUTER_BOUND('',#2782,.T.);
#1937=FACE_OUTER_BOUND('',#2783,.T.);
#1938=FACE_OUTER_BOUND('',#2784,.T.);
#1939=FACE_OUTER_BOUND('',#2785,.T.);
#1940=FACE_OUTER_BOUND('',#2786,.T.);
#1941=FACE_OUTER_BOUND('',#2788,.T.);
#1942=FACE_OUTER_BOUND('',#2789,.T.);
#1943=FACE_OUTER_BOUND('',#2790,.T.);
#1944=FACE_OUTER_BOUND('',#2791,.T.);
#1945=FACE_OUTER_BOUND('',#2792,.T.);
#1946=FACE_OUTER_BOUND('',#2793,.T.);
#1947=FACE_OUTER_BOUND('',#2794,.T.);
#1948=FACE_OUTER_BOUND('',#2795,.T.);
#1949=FACE_OUTER_BOUND('',#2796,.T.);
#1950=FACE_OUTER_BOUND('',#2797,.T.);
#1951=FACE_OUTER_BOUND('',#2798,.T.);
#1952=FACE_OUTER_BOUND('',#2799,.T.);
#1953=FACE_OUTER_BOUND('',#2800,.T.);
#1954=FACE_OUTER_BOUND('',#2801,.T.);
#1955=FACE_OUTER_BOUND('',#2802,.T.);
#1956=FACE_OUTER_BOUND('',#2803,.T.);
#1957=FACE_OUTER_BOUND('',#2804,.T.);
#1958=FACE_OUTER_BOUND('',#2806,.T.);
#1959=FACE_OUTER_BOUND('',#2807,.T.);
#1960=FACE_OUTER_BOUND('',#2808,.T.);
#1961=FACE_OUTER_BOUND('',#2809,.T.);
#1962=FACE_OUTER_BOUND('',#2810,.T.);
#1963=FACE_OUTER_BOUND('',#2811,.T.);
#1964=FACE_OUTER_BOUND('',#2812,.T.);
#1965=FACE_OUTER_BOUND('',#2813,.T.);
#1966=FACE_OUTER_BOUND('',#2814,.T.);
#1967=FACE_OUTER_BOUND('',#2815,.T.);
#1968=FACE_OUTER_BOUND('',#2816,.T.);
#1969=FACE_OUTER_BOUND('',#2817,.T.);
#1970=FACE_OUTER_BOUND('',#2818,.T.);
#1971=FACE_OUTER_BOUND('',#2819,.T.);
#1972=FACE_OUTER_BOUND('',#2820,.T.);
#1973=FACE_OUTER_BOUND('',#2822,.T.);
#1974=EDGE_LOOP('',(#8324,#8325,#8326,#8327));
#1975=EDGE_LOOP('',(#8328,#8329,#8330,#8331));
#1976=EDGE_LOOP('',(#8332,#8333,#8334,#8335));
#1977=EDGE_LOOP('',(#8336,#8337,#8338,#8339));
#1978=EDGE_LOOP('',(#8340,#8341,#8342,#8343));
#1979=EDGE_LOOP('',(#8344,#8345,#8346,#8347));
#1980=EDGE_LOOP('',(#8348,#8349,#8350,#8351));
#1981=EDGE_LOOP('',(#8352,#8353,#8354,#8355));
#1982=EDGE_LOOP('',(#8356,#8357,#8358,#8359));
#1983=EDGE_LOOP('',(#8360,#8361,#8362,#8363));
#1984=EDGE_LOOP('',(#8364,#8365,#8366,#8367));
#1985=EDGE_LOOP('',(#8368,#8369,#8370,#8371));
#1986=EDGE_LOOP('',(#8372,#8373,#8374,#8375));
#1987=EDGE_LOOP('',(#8376,#8377,#8378,#8379));
#1988=EDGE_LOOP('',(#8380,#8381,#8382,#8383));
#1989=EDGE_LOOP('',(#8384));
#1990=EDGE_LOOP('',(#8385));
#1991=EDGE_LOOP('',(#8386));
#1992=EDGE_LOOP('',(#8387));
#1993=EDGE_LOOP('',(#8388));
#1994=EDGE_LOOP('',(#8389));
#1995=EDGE_LOOP('',(#8390));
#1996=EDGE_LOOP('',(#8391));
#1997=EDGE_LOOP('',(#8392));
#1998=EDGE_LOOP('',(#8393));
#1999=EDGE_LOOP('',(#8394,#8395,#8396,#8397));
#2000=EDGE_LOOP('',(#8398));
#2001=EDGE_LOOP('',(#8399));
#2002=EDGE_LOOP('',(#8400));
#2003=EDGE_LOOP('',(#8401));
#2004=EDGE_LOOP('',(#8402));
#2005=EDGE_LOOP('',(#8403));
#2006=EDGE_LOOP('',(#8404));
#2007=EDGE_LOOP('',(#8405));
#2008=EDGE_LOOP('',(#8406));
#2009=EDGE_LOOP('',(#8407));
#2010=EDGE_LOOP('',(#8408,#8409,#8410,#8411));
#2011=EDGE_LOOP('',(#8412,#8413,#8414,#8415));
#2012=EDGE_LOOP('',(#8416,#8417,#8418,#8419));
#2013=EDGE_LOOP('',(#8420,#8421,#8422,#8423));
#2014=EDGE_LOOP('',(#8424,#8425,#8426,#8427));
#2015=EDGE_LOOP('',(#8428,#8429,#8430,#8431));
#2016=EDGE_LOOP('',(#8432,#8433,#8434,#8435));
#2017=EDGE_LOOP('',(#8436,#8437,#8438,#8439));
#2018=EDGE_LOOP('',(#8440,#8441,#8442,#8443));
#2019=EDGE_LOOP('',(#8444,#8445,#8446,#8447));
#2020=EDGE_LOOP('',(#8448,#8449,#8450,#8451));
#2021=EDGE_LOOP('',(#8452,#8453,#8454,#8455));
#2022=EDGE_LOOP('',(#8456,#8457,#8458,#8459));
#2023=EDGE_LOOP('',(#8460));
#2024=EDGE_LOOP('',(#8461,#8462,#8463,#8464));
#2025=EDGE_LOOP('',(#8465));
#2026=EDGE_LOOP('',(#8466,#8467,#8468,#8469));
#2027=EDGE_LOOP('',(#8470,#8471,#8472,#8473));
#2028=EDGE_LOOP('',(#8474,#8475,#8476,#8477,#8478,#8479,#8480,#8481));
#2029=EDGE_LOOP('',(#8482,#8483,#8484,#8485));
#2030=EDGE_LOOP('',(#8486,#8487,#8488,#8489));
#2031=EDGE_LOOP('',(#8490,#8491,#8492,#8493));
#2032=EDGE_LOOP('',(#8494,#8495,#8496,#8497,#8498,#8499,#8500,#8501));
#2033=EDGE_LOOP('',(#8502));
#2034=EDGE_LOOP('',(#8503));
#2035=EDGE_LOOP('',(#8504,#8505,#8506,#8507));
#2036=EDGE_LOOP('',(#8508,#8509,#8510,#8511));
#2037=EDGE_LOOP('',(#8512,#8513,#8514,#8515));
#2038=EDGE_LOOP('',(#8516));
#2039=EDGE_LOOP('',(#8517,#8518,#8519,#8520));
#2040=EDGE_LOOP('',(#8521));
#2041=EDGE_LOOP('',(#8522,#8523,#8524,#8525));
#2042=EDGE_LOOP('',(#8526,#8527,#8528,#8529));
#2043=EDGE_LOOP('',(#8530,#8531,#8532,#8533,#8534,#8535,#8536,#8537));
#2044=EDGE_LOOP('',(#8538,#8539,#8540,#8541));
#2045=EDGE_LOOP('',(#8542,#8543,#8544,#8545));
#2046=EDGE_LOOP('',(#8546,#8547,#8548,#8549));
#2047=EDGE_LOOP('',(#8550,#8551,#8552,#8553,#8554,#8555,#8556,#8557));
#2048=EDGE_LOOP('',(#8558));
#2049=EDGE_LOOP('',(#8559));
#2050=EDGE_LOOP('',(#8560,#8561,#8562,#8563));
#2051=EDGE_LOOP('',(#8564,#8565,#8566,#8567));
#2052=EDGE_LOOP('',(#8568,#8569,#8570,#8571));
#2053=EDGE_LOOP('',(#8572,#8573,#8574,#8575));
#2054=EDGE_LOOP('',(#8576,#8577,#8578,#8579));
#2055=EDGE_LOOP('',(#8580,#8581,#8582,#8583));
#2056=EDGE_LOOP('',(#8584,#8585,#8586,#8587));
#2057=EDGE_LOOP('',(#8588,#8589,#8590,#8591));
#2058=EDGE_LOOP('',(#8592));
#2059=EDGE_LOOP('',(#8593));
#2060=EDGE_LOOP('',(#8594));
#2061=EDGE_LOOP('',(#8595));
#2062=EDGE_LOOP('',(#8596,#8597,#8598,#8599));
#2063=EDGE_LOOP('',(#8600,#8601,#8602,#8603));
#2064=EDGE_LOOP('',(#8604,#8605,#8606,#8607));
#2065=EDGE_LOOP('',(#8608,#8609,#8610,#8611));
#2066=EDGE_LOOP('',(#8612,#8613,#8614,#8615));
#2067=EDGE_LOOP('',(#8616,#8617,#8618,#8619));
#2068=EDGE_LOOP('',(#8620,#8621,#8622,#8623));
#2069=EDGE_LOOP('',(#8624,#8625,#8626,#8627));
#2070=EDGE_LOOP('',(#8628,#8629,#8630,#8631));
#2071=EDGE_LOOP('',(#8632,#8633,#8634,#8635));
#2072=EDGE_LOOP('',(#8636,#8637,#8638,#8639));
#2073=EDGE_LOOP('',(#8640,#8641,#8642,#8643));
#2074=EDGE_LOOP('',(#8644));
#2075=EDGE_LOOP('',(#8645));
#2076=EDGE_LOOP('',(#8646));
#2077=EDGE_LOOP('',(#8647));
#2078=EDGE_LOOP('',(#8648,#8649,#8650,#8651));
#2079=EDGE_LOOP('',(#8652,#8653,#8654,#8655));
#2080=EDGE_LOOP('',(#8656,#8657,#8658,#8659,#8660,#8661));
#2081=EDGE_LOOP('',(#8662,#8663,#8664,#8665,#8666,#8667));
#2082=EDGE_LOOP('',(#8668,#8669,#8670,#8671,#8672,#8673));
#2083=EDGE_LOOP('',(#8674,#8675,#8676,#8677));
#2084=EDGE_LOOP('',(#8678,#8679,#8680,#8681));
#2085=EDGE_LOOP('',(#8682,#8683,#8684,#8685));
#2086=EDGE_LOOP('',(#8686,#8687,#8688,#8689));
#2087=EDGE_LOOP('',(#8690,#8691,#8692,#8693,#8694,#8695));
#2088=EDGE_LOOP('',(#8696,#8697,#8698,#8699));
#2089=EDGE_LOOP('',(#8700,#8701,#8702,#8703));
#2090=EDGE_LOOP('',(#8704,#8705,#8706,#8707));
#2091=EDGE_LOOP('',(#8708,#8709,#8710,#8711));
#2092=EDGE_LOOP('',(#8712,#8713,#8714,#8715));
#2093=EDGE_LOOP('',(#8716,#8717,#8718,#8719));
#2094=EDGE_LOOP('',(#8720,#8721,#8722,#8723));
#2095=EDGE_LOOP('',(#8724,#8725,#8726,#8727));
#2096=EDGE_LOOP('',(#8728,#8729,#8730,#8731,#8732,#8733,#8734,#8735,#8736,
#8737));
#2097=EDGE_LOOP('',(#8738));
#2098=EDGE_LOOP('',(#8739));
#2099=EDGE_LOOP('',(#8740,#8741,#8742,#8743));
#2100=EDGE_LOOP('',(#8744,#8745,#8746,#8747));
#2101=EDGE_LOOP('',(#8748,#8749,#8750,#8751));
#2102=EDGE_LOOP('',(#8752,#8753,#8754,#8755));
#2103=EDGE_LOOP('',(#8756,#8757,#8758,#8759,#8760,#8761,#8762,#8763,#8764,
#8765));
#2104=EDGE_LOOP('',(#8766));
#2105=EDGE_LOOP('',(#8767));
#2106=EDGE_LOOP('',(#8768,#8769,#8770,#8771));
#2107=EDGE_LOOP('',(#8772,#8773,#8774,#8775));
#2108=EDGE_LOOP('',(#8776,#8777,#8778,#8779,#8780,#8781));
#2109=EDGE_LOOP('',(#8782,#8783,#8784,#8785,#8786,#8787));
#2110=EDGE_LOOP('',(#8788,#8789,#8790,#8791,#8792,#8793));
#2111=EDGE_LOOP('',(#8794,#8795,#8796,#8797));
#2112=EDGE_LOOP('',(#8798,#8799,#8800,#8801));
#2113=EDGE_LOOP('',(#8802,#8803,#8804,#8805));
#2114=EDGE_LOOP('',(#8806,#8807,#8808,#8809));
#2115=EDGE_LOOP('',(#8810,#8811,#8812,#8813,#8814,#8815));
#2116=EDGE_LOOP('',(#8816,#8817,#8818,#8819));
#2117=EDGE_LOOP('',(#8820,#8821,#8822,#8823));
#2118=EDGE_LOOP('',(#8824,#8825,#8826,#8827));
#2119=EDGE_LOOP('',(#8828,#8829,#8830,#8831));
#2120=EDGE_LOOP('',(#8832,#8833,#8834,#8835));
#2121=EDGE_LOOP('',(#8836,#8837,#8838,#8839));
#2122=EDGE_LOOP('',(#8840,#8841,#8842,#8843));
#2123=EDGE_LOOP('',(#8844,#8845,#8846,#8847));
#2124=EDGE_LOOP('',(#8848,#8849,#8850,#8851,#8852,#8853,#8854,#8855,#8856,
#8857));
#2125=EDGE_LOOP('',(#8858));
#2126=EDGE_LOOP('',(#8859));
#2127=EDGE_LOOP('',(#8860,#8861,#8862,#8863));
#2128=EDGE_LOOP('',(#8864,#8865,#8866,#8867));
#2129=EDGE_LOOP('',(#8868,#8869,#8870,#8871));
#2130=EDGE_LOOP('',(#8872,#8873,#8874,#8875));
#2131=EDGE_LOOP('',(#8876,#8877,#8878,#8879,#8880,#8881,#8882,#8883,#8884,
#8885));
#2132=EDGE_LOOP('',(#8886));
#2133=EDGE_LOOP('',(#8887));
#2134=EDGE_LOOP('',(#8888,#8889,#8890,#8891));
#2135=EDGE_LOOP('',(#8892));
#2136=EDGE_LOOP('',(#8893));
#2137=EDGE_LOOP('',(#8894,#8895,#8896,#8897));
#2138=EDGE_LOOP('',(#8898));
#2139=EDGE_LOOP('',(#8899));
#2140=EDGE_LOOP('',(#8900,#8901,#8902,#8903));
#2141=EDGE_LOOP('',(#8904,#8905,#8906,#8907));
#2142=EDGE_LOOP('',(#8908,#8909,#8910,#8911));
#2143=EDGE_LOOP('',(#8912));
#2144=EDGE_LOOP('',(#8913));
#2145=EDGE_LOOP('',(#8914));
#2146=EDGE_LOOP('',(#8915));
#2147=EDGE_LOOP('',(#8916));
#2148=EDGE_LOOP('',(#8917));
#2149=EDGE_LOOP('',(#8918,#8919,#8920,#8921));
#2150=EDGE_LOOP('',(#8922,#8923,#8924,#8925,#8926));
#2151=EDGE_LOOP('',(#8927));
#2152=EDGE_LOOP('',(#8928));
#2153=EDGE_LOOP('',(#8929,#8930,#8931,#8932));
#2154=EDGE_LOOP('',(#8933,#8934,#8935,#8936));
#2155=EDGE_LOOP('',(#8937,#8938,#8939,#8940));
#2156=EDGE_LOOP('',(#8941,#8942,#8943,#8944));
#2157=EDGE_LOOP('',(#8945,#8946,#8947,#8948));
#2158=EDGE_LOOP('',(#8949,#8950,#8951,#8952));
#2159=EDGE_LOOP('',(#8953,#8954,#8955,#8956));
#2160=EDGE_LOOP('',(#8957,#8958,#8959,#8960));
#2161=EDGE_LOOP('',(#8961,#8962,#8963,#8964,#8965));
#2162=EDGE_LOOP('',(#8966));
#2163=EDGE_LOOP('',(#8967,#8968,#8969,#8970));
#2164=EDGE_LOOP('',(#8971));
#2165=EDGE_LOOP('',(#8972,#8973,#8974,#8975));
#2166=EDGE_LOOP('',(#8976,#8977,#8978,#8979,#8980,#8981,#8982,#8983));
#2167=EDGE_LOOP('',(#8984));
#2168=EDGE_LOOP('',(#8985));
#2169=EDGE_LOOP('',(#8986));
#2170=EDGE_LOOP('',(#8987));
#2171=EDGE_LOOP('',(#8988));
#2172=EDGE_LOOP('',(#8989,#8990,#8991,#8992));
#2173=EDGE_LOOP('',(#8993,#8994,#8995,#8996,#8997,#8998,#8999,#9000));
#2174=EDGE_LOOP('',(#9001));
#2175=EDGE_LOOP('',(#9002));
#2176=EDGE_LOOP('',(#9003));
#2177=EDGE_LOOP('',(#9004));
#2178=EDGE_LOOP('',(#9005));
#2179=EDGE_LOOP('',(#9006,#9007,#9008,#9009));
#2180=EDGE_LOOP('',(#9010,#9011,#9012,#9013));
#2181=EDGE_LOOP('',(#9014,#9015,#9016,#9017));
#2182=EDGE_LOOP('',(#9018,#9019,#9020,#9021));
#2183=EDGE_LOOP('',(#9022,#9023,#9024,#9025));
#2184=EDGE_LOOP('',(#9026,#9027,#9028,#9029));
#2185=EDGE_LOOP('',(#9030,#9031,#9032,#9033));
#2186=EDGE_LOOP('',(#9034,#9035,#9036,#9037));
#2187=EDGE_LOOP('',(#9038));
#2188=EDGE_LOOP('',(#9039));
#2189=EDGE_LOOP('',(#9040,#9041,#9042,#9043));
#2190=EDGE_LOOP('',(#9044));
#2191=EDGE_LOOP('',(#9045));
#2192=EDGE_LOOP('',(#9046));
#2193=EDGE_LOOP('',(#9047));
#2194=EDGE_LOOP('',(#9048));
#2195=EDGE_LOOP('',(#9049));
#2196=EDGE_LOOP('',(#9050));
#2197=EDGE_LOOP('',(#9051));
#2198=EDGE_LOOP('',(#9052));
#2199=EDGE_LOOP('',(#9053));
#2200=EDGE_LOOP('',(#9054));
#2201=EDGE_LOOP('',(#9055));
#2202=EDGE_LOOP('',(#9056,#9057,#9058,#9059));
#2203=EDGE_LOOP('',(#9060,#9061,#9062,#9063));
#2204=EDGE_LOOP('',(#9064,#9065,#9066,#9067));
#2205=EDGE_LOOP('',(#9068,#9069,#9070,#9071));
#2206=EDGE_LOOP('',(#9072,#9073,#9074,#9075));
#2207=EDGE_LOOP('',(#9076,#9077,#9078,#9079));
#2208=EDGE_LOOP('',(#9080));
#2209=EDGE_LOOP('',(#9081));
#2210=EDGE_LOOP('',(#9082,#9083,#9084,#9085));
#2211=EDGE_LOOP('',(#9086));
#2212=EDGE_LOOP('',(#9087));
#2213=EDGE_LOOP('',(#9088));
#2214=EDGE_LOOP('',(#9089));
#2215=EDGE_LOOP('',(#9090));
#2216=EDGE_LOOP('',(#9091));
#2217=EDGE_LOOP('',(#9092));
#2218=EDGE_LOOP('',(#9093));
#2219=EDGE_LOOP('',(#9094));
#2220=EDGE_LOOP('',(#9095));
#2221=EDGE_LOOP('',(#9096));
#2222=EDGE_LOOP('',(#9097));
#2223=EDGE_LOOP('',(#9098,#9099,#9100,#9101));
#2224=EDGE_LOOP('',(#9102,#9103,#9104,#9105,#9106));
#2225=EDGE_LOOP('',(#9107));
#2226=EDGE_LOOP('',(#9108));
#2227=EDGE_LOOP('',(#9109,#9110,#9111,#9112,#9113,#9114,#9115,#9116));
#2228=EDGE_LOOP('',(#9117));
#2229=EDGE_LOOP('',(#9118));
#2230=EDGE_LOOP('',(#9119));
#2231=EDGE_LOOP('',(#9120));
#2232=EDGE_LOOP('',(#9121));
#2233=EDGE_LOOP('',(#9122,#9123,#9124,#9125));
#2234=EDGE_LOOP('',(#9126,#9127,#9128,#9129));
#2235=EDGE_LOOP('',(#9130,#9131,#9132,#9133));
#2236=EDGE_LOOP('',(#9134,#9135,#9136,#9137));
#2237=EDGE_LOOP('',(#9138,#9139,#9140,#9141));
#2238=EDGE_LOOP('',(#9142,#9143,#9144,#9145));
#2239=EDGE_LOOP('',(#9146,#9147,#9148,#9149));
#2240=EDGE_LOOP('',(#9150,#9151,#9152,#9153,#9154));
#2241=EDGE_LOOP('',(#9155));
#2242=EDGE_LOOP('',(#9156,#9157,#9158,#9159));
#2243=EDGE_LOOP('',(#9160));
#2244=EDGE_LOOP('',(#9161,#9162,#9163,#9164));
#2245=EDGE_LOOP('',(#9165,#9166,#9167,#9168));
#2246=EDGE_LOOP('',(#9169,#9170,#9171,#9172));
#2247=EDGE_LOOP('',(#9173,#9174,#9175,#9176,#9177,#9178,#9179,#9180));
#2248=EDGE_LOOP('',(#9181));
#2249=EDGE_LOOP('',(#9182));
#2250=EDGE_LOOP('',(#9183));
#2251=EDGE_LOOP('',(#9184));
#2252=EDGE_LOOP('',(#9185));
#2253=EDGE_LOOP('',(#9186,#9187,#9188,#9189));
#2254=EDGE_LOOP('',(#9190,#9191,#9192,#9193));
#2255=EDGE_LOOP('',(#9194,#9195,#9196,#9197));
#2256=EDGE_LOOP('',(#9198,#9199,#9200,#9201));
#2257=EDGE_LOOP('',(#9202,#9203,#9204,#9205));
#2258=EDGE_LOOP('',(#9206,#9207,#9208,#9209));
#2259=EDGE_LOOP('',(#9210,#9211,#9212,#9213));
#2260=EDGE_LOOP('',(#9214,#9215,#9216,#9217));
#2261=EDGE_LOOP('',(#9218));
#2262=EDGE_LOOP('',(#9219));
#2263=EDGE_LOOP('',(#9220,#9221,#9222,#9223));
#2264=EDGE_LOOP('',(#9224));
#2265=EDGE_LOOP('',(#9225));
#2266=EDGE_LOOP('',(#9226));
#2267=EDGE_LOOP('',(#9227));
#2268=EDGE_LOOP('',(#9228));
#2269=EDGE_LOOP('',(#9229));
#2270=EDGE_LOOP('',(#9230));
#2271=EDGE_LOOP('',(#9231));
#2272=EDGE_LOOP('',(#9232));
#2273=EDGE_LOOP('',(#9233));
#2274=EDGE_LOOP('',(#9234));
#2275=EDGE_LOOP('',(#9235));
#2276=EDGE_LOOP('',(#9236,#9237,#9238,#9239));
#2277=EDGE_LOOP('',(#9240,#9241,#9242,#9243));
#2278=EDGE_LOOP('',(#9244,#9245,#9246,#9247));
#2279=EDGE_LOOP('',(#9248,#9249,#9250,#9251));
#2280=EDGE_LOOP('',(#9252,#9253,#9254,#9255));
#2281=EDGE_LOOP('',(#9256,#9257,#9258,#9259));
#2282=EDGE_LOOP('',(#9260));
#2283=EDGE_LOOP('',(#9261));
#2284=EDGE_LOOP('',(#9262,#9263,#9264,#9265));
#2285=EDGE_LOOP('',(#9266));
#2286=EDGE_LOOP('',(#9267));
#2287=EDGE_LOOP('',(#9268));
#2288=EDGE_LOOP('',(#9269));
#2289=EDGE_LOOP('',(#9270));
#2290=EDGE_LOOP('',(#9271));
#2291=EDGE_LOOP('',(#9272));
#2292=EDGE_LOOP('',(#9273));
#2293=EDGE_LOOP('',(#9274));
#2294=EDGE_LOOP('',(#9275));
#2295=EDGE_LOOP('',(#9276));
#2296=EDGE_LOOP('',(#9277));
#2297=EDGE_LOOP('',(#9278));
#2298=EDGE_LOOP('',(#9279,#9280,#9281,#9282));
#2299=EDGE_LOOP('',(#9283,#9284,#9285,#9286));
#2300=EDGE_LOOP('',(#9287,#9288,#9289,#9290));
#2301=EDGE_LOOP('',(#9291));
#2302=EDGE_LOOP('',(#9292));
#2303=EDGE_LOOP('',(#9293,#9294,#9295,#9296));
#2304=EDGE_LOOP('',(#9297,#9298,#9299,#9300));
#2305=EDGE_LOOP('',(#9301,#9302,#9303,#9304));
#2306=EDGE_LOOP('',(#9305));
#2307=EDGE_LOOP('',(#9306,#9307,#9308,#9309));
#2308=EDGE_LOOP('',(#9310,#9311,#9312,#9313));
#2309=EDGE_LOOP('',(#9314,#9315,#9316,#9317));
#2310=EDGE_LOOP('',(#9318,#9319,#9320,#9321));
#2311=EDGE_LOOP('',(#9322,#9323,#9324,#9325));
#2312=EDGE_LOOP('',(#9326,#9327,#9328,#9329));
#2313=EDGE_LOOP('',(#9330,#9331,#9332,#9333,#9334,#9335));
#2314=EDGE_LOOP('',(#9336,#9337,#9338,#9339,#9340,#9341));
#2315=EDGE_LOOP('',(#9342,#9343,#9344,#9345,#9346,#9347));
#2316=EDGE_LOOP('',(#9348,#9349,#9350,#9351,#9352));
#2317=EDGE_LOOP('',(#9353,#9354,#9355,#9356));
#2318=EDGE_LOOP('',(#9357,#9358,#9359,#9360));
#2319=EDGE_LOOP('',(#9361));
#2320=EDGE_LOOP('',(#9362));
#2321=EDGE_LOOP('',(#9363,#9364,#9365,#9366,#9367));
#2322=EDGE_LOOP('',(#9368));
#2323=EDGE_LOOP('',(#9369));
#2324=EDGE_LOOP('',(#9370,#9371,#9372,#9373));
#2325=EDGE_LOOP('',(#9374,#9375,#9376,#9377,#9378,#9379));
#2326=EDGE_LOOP('',(#9380,#9381,#9382,#9383,#9384));
#2327=EDGE_LOOP('',(#9385));
#2328=EDGE_LOOP('',(#9386));
#2329=EDGE_LOOP('',(#9387,#9388,#9389,#9390));
#2330=EDGE_LOOP('',(#9391,#9392,#9393,#9394));
#2331=EDGE_LOOP('',(#9395,#9396,#9397,#9398));
#2332=EDGE_LOOP('',(#9399));
#2333=EDGE_LOOP('',(#9400));
#2334=EDGE_LOOP('',(#9401,#9402,#9403,#9404,#9405));
#2335=EDGE_LOOP('',(#9406,#9407));
#2336=EDGE_LOOP('',(#9408,#9409));
#2337=EDGE_LOOP('',(#9410,#9411));
#2338=EDGE_LOOP('',(#9412,#9413));
#2339=EDGE_LOOP('',(#9414,#9415));
#2340=EDGE_LOOP('',(#9416,#9417));
#2341=EDGE_LOOP('',(#9418,#9419));
#2342=EDGE_LOOP('',(#9420,#9421,#9422,#9423));
#2343=EDGE_LOOP('',(#9424,#9425,#9426,#9427,#9428,#9429,#9430,#9431,#9432,
#9433,#9434,#9435,#9436,#9437,#9438,#9439,#9440,#9441));
#2344=EDGE_LOOP('',(#9442,#9443,#9444,#9445));
#2345=EDGE_LOOP('',(#9446,#9447,#9448,#9449));
#2346=EDGE_LOOP('',(#9450,#9451,#9452,#9453));
#2347=EDGE_LOOP('',(#9454,#9455,#9456,#9457));
#2348=EDGE_LOOP('',(#9458,#9459,#9460,#9461,#9462,#9463));
#2349=EDGE_LOOP('',(#9464,#9465,#9466,#9467));
#2350=EDGE_LOOP('',(#9468,#9469,#9470,#9471));
#2351=EDGE_LOOP('',(#9472,#9473,#9474,#9475));
#2352=EDGE_LOOP('',(#9476,#9477,#9478,#9479));
#2353=EDGE_LOOP('',(#9480,#9481,#9482,#9483));
#2354=EDGE_LOOP('',(#9484,#9485,#9486,#9487,#9488,#9489,#9490,#9491,#9492,
#9493,#9494,#9495,#9496,#9497,#9498,#9499,#9500,#9501));
#2355=EDGE_LOOP('',(#9502,#9503,#9504,#9505));
#2356=EDGE_LOOP('',(#9506,#9507,#9508,#9509));
#2357=EDGE_LOOP('',(#9510));
#2358=EDGE_LOOP('',(#9511));
#2359=EDGE_LOOP('',(#9512,#9513,#9514,#9515));
#2360=EDGE_LOOP('',(#9516));
#2361=EDGE_LOOP('',(#9517));
#2362=EDGE_LOOP('',(#9518,#9519,#9520,#9521));
#2363=EDGE_LOOP('',(#9522));
#2364=EDGE_LOOP('',(#9523));
#2365=EDGE_LOOP('',(#9524,#9525,#9526,#9527));
#2366=EDGE_LOOP('',(#9528));
#2367=EDGE_LOOP('',(#9529));
#2368=EDGE_LOOP('',(#9530,#9531,#9532,#9533));
#2369=EDGE_LOOP('',(#9534));
#2370=EDGE_LOOP('',(#9535));
#2371=EDGE_LOOP('',(#9536,#9537,#9538,#9539));
#2372=EDGE_LOOP('',(#9540,#9541,#9542,#9543));
#2373=EDGE_LOOP('',(#9544,#9545,#9546,#9547));
#2374=EDGE_LOOP('',(#9548,#9549,#9550,#9551));
#2375=EDGE_LOOP('',(#9552,#9553,#9554,#9555));
#2376=EDGE_LOOP('',(#9556,#9557,#9558,#9559));
#2377=EDGE_LOOP('',(#9560,#9561,#9562,#9563));
#2378=EDGE_LOOP('',(#9564,#9565,#9566,#9567,#9568,#9569));
#2379=EDGE_LOOP('',(#9570,#9571,#9572,#9573,#9574,#9575));
#2380=EDGE_LOOP('',(#9576));
#2381=EDGE_LOOP('',(#9577));
#2382=EDGE_LOOP('',(#9578,#9579,#9580,#9581));
#2383=EDGE_LOOP('',(#9582,#9583,#9584,#9585));
#2384=EDGE_LOOP('',(#9586,#9587,#9588,#9589));
#2385=EDGE_LOOP('',(#9590));
#2386=EDGE_LOOP('',(#9591));
#2387=EDGE_LOOP('',(#9592,#9593,#9594,#9595));
#2388=EDGE_LOOP('',(#9596,#9597,#9598,#9599));
#2389=EDGE_LOOP('',(#9600,#9601,#9602,#9603));
#2390=EDGE_LOOP('',(#9604));
#2391=EDGE_LOOP('',(#9605,#9606,#9607,#9608));
#2392=EDGE_LOOP('',(#9609,#9610,#9611,#9612));
#2393=EDGE_LOOP('',(#9613,#9614,#9615,#9616,#9617,#9618,#9619));
#2394=EDGE_LOOP('',(#9620,#9621,#9622,#9623,#9624,#9625,#9626));
#2395=EDGE_LOOP('',(#9627,#9628,#9629,#9630));
#2396=EDGE_LOOP('',(#9631,#9632,#9633,#9634));
#2397=EDGE_LOOP('',(#9635,#9636,#9637,#9638));
#2398=EDGE_LOOP('',(#9639,#9640,#9641,#9642));
#2399=EDGE_LOOP('',(#9643,#9644,#9645,#9646));
#2400=EDGE_LOOP('',(#9647,#9648,#9649,#9650));
#2401=EDGE_LOOP('',(#9651,#9652,#9653,#9654));
#2402=EDGE_LOOP('',(#9655,#9656,#9657,#9658));
#2403=EDGE_LOOP('',(#9659,#9660,#9661,#9662));
#2404=EDGE_LOOP('',(#9663,#9664,#9665,#9666));
#2405=EDGE_LOOP('',(#9667,#9668,#9669,#9670));
#2406=EDGE_LOOP('',(#9671,#9672,#9673,#9674));
#2407=EDGE_LOOP('',(#9675,#9676,#9677,#9678));
#2408=EDGE_LOOP('',(#9679,#9680,#9681,#9682));
#2409=EDGE_LOOP('',(#9683,#9684,#9685,#9686));
#2410=EDGE_LOOP('',(#9687,#9688,#9689,#9690));
#2411=EDGE_LOOP('',(#9691,#9692,#9693,#9694));
#2412=EDGE_LOOP('',(#9695,#9696,#9697,#9698));
#2413=EDGE_LOOP('',(#9699,#9700,#9701,#9702));
#2414=EDGE_LOOP('',(#9703,#9704,#9705,#9706));
#2415=EDGE_LOOP('',(#9707,#9708,#9709,#9710));
#2416=EDGE_LOOP('',(#9711,#9712,#9713,#9714));
#2417=EDGE_LOOP('',(#9715,#9716,#9717,#9718));
#2418=EDGE_LOOP('',(#9719,#9720,#9721,#9722));
#2419=EDGE_LOOP('',(#9723,#9724,#9725,#9726));
#2420=EDGE_LOOP('',(#9727,#9728,#9729,#9730));
#2421=EDGE_LOOP('',(#9731,#9732,#9733,#9734));
#2422=EDGE_LOOP('',(#9735,#9736,#9737,#9738));
#2423=EDGE_LOOP('',(#9739,#9740,#9741,#9742));
#2424=EDGE_LOOP('',(#9743,#9744,#9745,#9746));
#2425=EDGE_LOOP('',(#9747,#9748,#9749,#9750));
#2426=EDGE_LOOP('',(#9751,#9752,#9753,#9754));
#2427=EDGE_LOOP('',(#9755,#9756,#9757,#9758));
#2428=EDGE_LOOP('',(#9759,#9760,#9761,#9762));
#2429=EDGE_LOOP('',(#9763,#9764,#9765,#9766));
#2430=EDGE_LOOP('',(#9767,#9768,#9769,#9770));
#2431=EDGE_LOOP('',(#9771,#9772,#9773,#9774));
#2432=EDGE_LOOP('',(#9775,#9776,#9777,#9778));
#2433=EDGE_LOOP('',(#9779,#9780,#9781,#9782));
#2434=EDGE_LOOP('',(#9783,#9784,#9785,#9786));
#2435=EDGE_LOOP('',(#9787,#9788,#9789,#9790));
#2436=EDGE_LOOP('',(#9791,#9792,#9793,#9794));
#2437=EDGE_LOOP('',(#9795,#9796,#9797,#9798));
#2438=EDGE_LOOP('',(#9799,#9800,#9801,#9802));
#2439=EDGE_LOOP('',(#9803,#9804,#9805,#9806));
#2440=EDGE_LOOP('',(#9807,#9808,#9809,#9810));
#2441=EDGE_LOOP('',(#9811,#9812,#9813,#9814));
#2442=EDGE_LOOP('',(#9815,#9816,#9817,#9818));
#2443=EDGE_LOOP('',(#9819,#9820,#9821,#9822));
#2444=EDGE_LOOP('',(#9823,#9824,#9825,#9826));
#2445=EDGE_LOOP('',(#9827,#9828,#9829,#9830));
#2446=EDGE_LOOP('',(#9831,#9832,#9833,#9834));
#2447=EDGE_LOOP('',(#9835,#9836,#9837,#9838));
#2448=EDGE_LOOP('',(#9839,#9840,#9841,#9842));
#2449=EDGE_LOOP('',(#9843,#9844,#9845,#9846));
#2450=EDGE_LOOP('',(#9847,#9848,#9849,#9850));
#2451=EDGE_LOOP('',(#9851,#9852,#9853,#9854));
#2452=EDGE_LOOP('',(#9855,#9856,#9857,#9858));
#2453=EDGE_LOOP('',(#9859,#9860,#9861,#9862));
#2454=EDGE_LOOP('',(#9863,#9864,#9865,#9866));
#2455=EDGE_LOOP('',(#9867,#9868,#9869,#9870));
#2456=EDGE_LOOP('',(#9871,#9872,#9873,#9874));
#2457=EDGE_LOOP('',(#9875,#9876,#9877,#9878));
#2458=EDGE_LOOP('',(#9879,#9880,#9881,#9882));
#2459=EDGE_LOOP('',(#9883,#9884,#9885,#9886));
#2460=EDGE_LOOP('',(#9887,#9888,#9889,#9890));
#2461=EDGE_LOOP('',(#9891,#9892,#9893,#9894));
#2462=EDGE_LOOP('',(#9895,#9896,#9897,#9898));
#2463=EDGE_LOOP('',(#9899,#9900,#9901,#9902));
#2464=EDGE_LOOP('',(#9903,#9904,#9905,#9906));
#2465=EDGE_LOOP('',(#9907,#9908,#9909,#9910));
#2466=EDGE_LOOP('',(#9911,#9912,#9913,#9914));
#2467=EDGE_LOOP('',(#9915,#9916,#9917,#9918));
#2468=EDGE_LOOP('',(#9919,#9920,#9921,#9922));
#2469=EDGE_LOOP('',(#9923,#9924,#9925,#9926));
#2470=EDGE_LOOP('',(#9927,#9928,#9929,#9930));
#2471=EDGE_LOOP('',(#9931,#9932,#9933,#9934));
#2472=EDGE_LOOP('',(#9935,#9936,#9937,#9938));
#2473=EDGE_LOOP('',(#9939,#9940,#9941,#9942));
#2474=EDGE_LOOP('',(#9943,#9944,#9945,#9946));
#2475=EDGE_LOOP('',(#9947,#9948,#9949,#9950));
#2476=EDGE_LOOP('',(#9951,#9952,#9953,#9954));
#2477=EDGE_LOOP('',(#9955,#9956,#9957,#9958));
#2478=EDGE_LOOP('',(#9959,#9960,#9961,#9962));
#2479=EDGE_LOOP('',(#9963,#9964,#9965,#9966));
#2480=EDGE_LOOP('',(#9967,#9968,#9969,#9970));
#2481=EDGE_LOOP('',(#9971,#9972,#9973,#9974));
#2482=EDGE_LOOP('',(#9975,#9976,#9977,#9978));
#2483=EDGE_LOOP('',(#9979,#9980,#9981,#9982));
#2484=EDGE_LOOP('',(#9983,#9984,#9985,#9986));
#2485=EDGE_LOOP('',(#9987,#9988,#9989,#9990));
#2486=EDGE_LOOP('',(#9991,#9992,#9993,#9994));
#2487=EDGE_LOOP('',(#9995,#9996,#9997,#9998));
#2488=EDGE_LOOP('',(#9999,#10000,#10001,#10002));
#2489=EDGE_LOOP('',(#10003,#10004,#10005,#10006));
#2490=EDGE_LOOP('',(#10007,#10008,#10009,#10010));
#2491=EDGE_LOOP('',(#10011,#10012,#10013,#10014));
#2492=EDGE_LOOP('',(#10015,#10016,#10017,#10018));
#2493=EDGE_LOOP('',(#10019,#10020,#10021,#10022));
#2494=EDGE_LOOP('',(#10023,#10024,#10025,#10026));
#2495=EDGE_LOOP('',(#10027,#10028,#10029,#10030));
#2496=EDGE_LOOP('',(#10031,#10032,#10033,#10034));
#2497=EDGE_LOOP('',(#10035,#10036,#10037,#10038));
#2498=EDGE_LOOP('',(#10039,#10040,#10041,#10042));
#2499=EDGE_LOOP('',(#10043,#10044,#10045,#10046));
#2500=EDGE_LOOP('',(#10047,#10048,#10049,#10050));
#2501=EDGE_LOOP('',(#10051,#10052,#10053,#10054));
#2502=EDGE_LOOP('',(#10055,#10056,#10057,#10058));
#2503=EDGE_LOOP('',(#10059,#10060,#10061,#10062));
#2504=EDGE_LOOP('',(#10063,#10064,#10065,#10066));
#2505=EDGE_LOOP('',(#10067,#10068,#10069,#10070));
#2506=EDGE_LOOP('',(#10071,#10072,#10073,#10074));
#2507=EDGE_LOOP('',(#10075,#10076,#10077,#10078));
#2508=EDGE_LOOP('',(#10079,#10080,#10081,#10082));
#2509=EDGE_LOOP('',(#10083,#10084,#10085,#10086));
#2510=EDGE_LOOP('',(#10087,#10088,#10089,#10090));
#2511=EDGE_LOOP('',(#10091,#10092,#10093,#10094));
#2512=EDGE_LOOP('',(#10095,#10096,#10097,#10098));
#2513=EDGE_LOOP('',(#10099,#10100,#10101,#10102));
#2514=EDGE_LOOP('',(#10103,#10104,#10105,#10106));
#2515=EDGE_LOOP('',(#10107,#10108,#10109,#10110));
#2516=EDGE_LOOP('',(#10111,#10112,#10113,#10114));
#2517=EDGE_LOOP('',(#10115,#10116,#10117,#10118));
#2518=EDGE_LOOP('',(#10119,#10120,#10121,#10122));
#2519=EDGE_LOOP('',(#10123,#10124,#10125,#10126));
#2520=EDGE_LOOP('',(#10127,#10128,#10129,#10130));
#2521=EDGE_LOOP('',(#10131,#10132,#10133,#10134));
#2522=EDGE_LOOP('',(#10135,#10136,#10137,#10138));
#2523=EDGE_LOOP('',(#10139,#10140,#10141,#10142));
#2524=EDGE_LOOP('',(#10143,#10144,#10145,#10146));
#2525=EDGE_LOOP('',(#10147,#10148,#10149,#10150));
#2526=EDGE_LOOP('',(#10151,#10152,#10153,#10154));
#2527=EDGE_LOOP('',(#10155,#10156,#10157,#10158));
#2528=EDGE_LOOP('',(#10159,#10160,#10161,#10162));
#2529=EDGE_LOOP('',(#10163,#10164,#10165,#10166));
#2530=EDGE_LOOP('',(#10167,#10168,#10169,#10170));
#2531=EDGE_LOOP('',(#10171,#10172,#10173,#10174));
#2532=EDGE_LOOP('',(#10175,#10176,#10177,#10178));
#2533=EDGE_LOOP('',(#10179,#10180,#10181,#10182));
#2534=EDGE_LOOP('',(#10183,#10184,#10185,#10186));
#2535=EDGE_LOOP('',(#10187,#10188,#10189,#10190));
#2536=EDGE_LOOP('',(#10191,#10192,#10193,#10194));
#2537=EDGE_LOOP('',(#10195,#10196,#10197,#10198));
#2538=EDGE_LOOP('',(#10199,#10200,#10201,#10202));
#2539=EDGE_LOOP('',(#10203,#10204,#10205,#10206));
#2540=EDGE_LOOP('',(#10207,#10208,#10209,#10210));
#2541=EDGE_LOOP('',(#10211,#10212,#10213,#10214));
#2542=EDGE_LOOP('',(#10215,#10216,#10217,#10218));
#2543=EDGE_LOOP('',(#10219,#10220,#10221,#10222));
#2544=EDGE_LOOP('',(#10223,#10224,#10225,#10226));
#2545=EDGE_LOOP('',(#10227,#10228,#10229,#10230));
#2546=EDGE_LOOP('',(#10231,#10232,#10233,#10234));
#2547=EDGE_LOOP('',(#10235,#10236,#10237,#10238));
#2548=EDGE_LOOP('',(#10239,#10240,#10241,#10242));
#2549=EDGE_LOOP('',(#10243,#10244,#10245,#10246));
#2550=EDGE_LOOP('',(#10247,#10248,#10249,#10250));
#2551=EDGE_LOOP('',(#10251,#10252,#10253,#10254));
#2552=EDGE_LOOP('',(#10255,#10256,#10257,#10258));
#2553=EDGE_LOOP('',(#10259,#10260,#10261,#10262));
#2554=EDGE_LOOP('',(#10263,#10264,#10265,#10266));
#2555=EDGE_LOOP('',(#10267,#10268,#10269,#10270));
#2556=EDGE_LOOP('',(#10271,#10272,#10273,#10274,#10275,#10276,#10277,#10278,
#10279,#10280,#10281,#10282,#10283,#10284,#10285,#10286,#10287,#10288,#10289,
#10290,#10291,#10292,#10293,#10294,#10295,#10296,#10297,#10298,#10299,#10300,
#10301,#10302,#10303,#10304,#10305,#10306,#10307,#10308,#10309,#10310,#10311,
#10312,#10313,#10314,#10315,#10316,#10317,#10318,#10319,#10320,#10321,#10322,
#10323,#10324,#10325,#10326,#10327,#10328,#10329,#10330,#10331,#10332,#10333,
#10334,#10335,#10336,#10337,#10338,#10339,#10340,#10341,#10342,#10343,#10344,
#10345,#10346,#10347,#10348,#10349,#10350,#10351,#10352,#10353,#10354,#10355,
#10356,#10357,#10358,#10359,#10360,#10361,#10362,#10363,#10364,#10365,#10366,
#10367,#10368,#10369,#10370,#10371,#10372,#10373,#10374,#10375,#10376,#10377,
#10378,#10379,#10380,#10381,#10382,#10383,#10384,#10385,#10386,#10387,#10388,
#10389,#10390,#10391,#10392,#10393,#10394,#10395,#10396,#10397,#10398,#10399,
#10400,#10401,#10402,#10403,#10404,#10405,#10406,#10407,#10408,#10409,#10410,
#10411,#10412,#10413,#10414,#10415,#10416,#10417,#10418,#10419,#10420,#10421,
#10422,#10423,#10424,#10425,#10426,#10427,#10428,#10429,#10430,#10431,#10432,
#10433,#10434));
#2557=EDGE_LOOP('',(#10435,#10436,#10437,#10438,#10439,#10440,#10441,#10442,
#10443,#10444,#10445,#10446,#10447,#10448,#10449,#10450,#10451,#10452,#10453,
#10454,#10455,#10456,#10457,#10458,#10459,#10460,#10461,#10462,#10463,#10464,
#10465,#10466,#10467,#10468,#10469,#10470,#10471,#10472,#10473,#10474,#10475,
#10476,#10477,#10478,#10479,#10480,#10481,#10482,#10483,#10484,#10485,#10486,
#10487,#10488,#10489,#10490,#10491,#10492,#10493,#10494,#10495,#10496,#10497,
#10498,#10499,#10500,#10501,#10502,#10503,#10504,#10505,#10506,#10507,#10508,
#10509,#10510,#10511,#10512,#10513,#10514,#10515,#10516,#10517,#10518,#10519,
#10520,#10521,#10522,#10523,#10524,#10525,#10526,#10527,#10528,#10529,#10530,
#10531,#10532,#10533,#10534,#10535,#10536,#10537,#10538,#10539,#10540,#10541,
#10542,#10543,#10544,#10545,#10546,#10547,#10548,#10549,#10550,#10551,#10552,
#10553,#10554,#10555,#10556,#10557,#10558,#10559,#10560,#10561,#10562,#10563,
#10564,#10565,#10566,#10567,#10568,#10569,#10570,#10571,#10572,#10573,#10574,
#10575,#10576,#10577,#10578,#10579,#10580,#10581,#10582,#10583,#10584,#10585,
#10586,#10587,#10588,#10589,#10590,#10591,#10592,#10593,#10594,#10595,#10596,
#10597,#10598));
#2558=EDGE_LOOP('',(#10599,#10600,#10601,#10602,#10603,#10604,#10605,#10606,
#10607,#10608,#10609,#10610));
#2559=EDGE_LOOP('',(#10611));
#2560=EDGE_LOOP('',(#10612));
#2561=EDGE_LOOP('',(#10613));
#2562=EDGE_LOOP('',(#10614,#10615,#10616,#10617));
#2563=EDGE_LOOP('',(#10618));
#2564=EDGE_LOOP('',(#10619,#10620,#10621,#10622));
#2565=EDGE_LOOP('',(#10623));
#2566=EDGE_LOOP('',(#10624));
#2567=EDGE_LOOP('',(#10625));
#2568=EDGE_LOOP('',(#10626,#10627,#10628,#10629,#10630,#10631));
#2569=EDGE_LOOP('',(#10632,#10633,#10634,#10635));
#2570=EDGE_LOOP('',(#10636,#10637,#10638,#10639));
#2571=EDGE_LOOP('',(#10640,#10641,#10642,#10643));
#2572=EDGE_LOOP('',(#10644,#10645,#10646,#10647));
#2573=EDGE_LOOP('',(#10648,#10649,#10650,#10651,#10652,#10653));
#2574=EDGE_LOOP('',(#10654,#10655,#10656,#10657));
#2575=EDGE_LOOP('',(#10658,#10659));
#2576=EDGE_LOOP('',(#10660,#10661,#10662,#10663));
#2577=EDGE_LOOP('',(#10664,#10665));
#2578=EDGE_LOOP('',(#10666,#10667,#10668,#10669,#10670,#10671));
#2579=EDGE_LOOP('',(#10672,#10673,#10674,#10675));
#2580=EDGE_LOOP('',(#10676,#10677,#10678,#10679));
#2581=EDGE_LOOP('',(#10680,#10681,#10682,#10683));
#2582=EDGE_LOOP('',(#10684,#10685,#10686,#10687));
#2583=EDGE_LOOP('',(#10688,#10689,#10690,#10691));
#2584=EDGE_LOOP('',(#10692,#10693,#10694,#10695));
#2585=EDGE_LOOP('',(#10696,#10697,#10698,#10699,#10700,#10701));
#2586=EDGE_LOOP('',(#10702));
#2587=EDGE_LOOP('',(#10703,#10704,#10705,#10706,#10707,#10708));
#2588=EDGE_LOOP('',(#10709,#10710,#10711,#10712));
#2589=EDGE_LOOP('',(#10713,#10714,#10715,#10716));
#2590=EDGE_LOOP('',(#10717,#10718,#10719,#10720));
#2591=EDGE_LOOP('',(#10721));
#2592=EDGE_LOOP('',(#10722,#10723,#10724,#10725));
#2593=EDGE_LOOP('',(#10726));
#2594=EDGE_LOOP('',(#10727,#10728,#10729,#10730));
#2595=EDGE_LOOP('',(#10731));
#2596=EDGE_LOOP('',(#10732,#10733,#10734,#10735));
#2597=EDGE_LOOP('',(#10736,#10737,#10738,#10739));
#2598=EDGE_LOOP('',(#10740,#10741,#10742,#10743));
#2599=EDGE_LOOP('',(#10744,#10745,#10746,#10747));
#2600=EDGE_LOOP('',(#10748,#10749,#10750,#10751));
#2601=EDGE_LOOP('',(#10752,#10753,#10754,#10755));
#2602=EDGE_LOOP('',(#10756,#10757,#10758,#10759));
#2603=EDGE_LOOP('',(#10760,#10761,#10762,#10763));
#2604=EDGE_LOOP('',(#10764,#10765,#10766,#10767));
#2605=EDGE_LOOP('',(#10768,#10769,#10770,#10771));
#2606=EDGE_LOOP('',(#10772,#10773,#10774,#10775));
#2607=EDGE_LOOP('',(#10776,#10777,#10778,#10779));
#2608=EDGE_LOOP('',(#10780,#10781,#10782,#10783));
#2609=EDGE_LOOP('',(#10784));
#2610=EDGE_LOOP('',(#10785));
#2611=EDGE_LOOP('',(#10786));
#2612=EDGE_LOOP('',(#10787));
#2613=EDGE_LOOP('',(#10788,#10789,#10790,#10791));
#2614=EDGE_LOOP('',(#10792,#10793,#10794,#10795));
#2615=EDGE_LOOP('',(#10796));
#2616=EDGE_LOOP('',(#10797));
#2617=EDGE_LOOP('',(#10798));
#2618=EDGE_LOOP('',(#10799));
#2619=EDGE_LOOP('',(#10800,#10801,#10802,#10803));
#2620=EDGE_LOOP('',(#10804,#10805,#10806,#10807));
#2621=EDGE_LOOP('',(#10808));
#2622=EDGE_LOOP('',(#10809));
#2623=EDGE_LOOP('',(#10810));
#2624=EDGE_LOOP('',(#10811));
#2625=EDGE_LOOP('',(#10812,#10813,#10814,#10815));
#2626=EDGE_LOOP('',(#10816,#10817,#10818,#10819));
#2627=EDGE_LOOP('',(#10820));
#2628=EDGE_LOOP('',(#10821));
#2629=EDGE_LOOP('',(#10822));
#2630=EDGE_LOOP('',(#10823));
#2631=EDGE_LOOP('',(#10824,#10825,#10826,#10827));
#2632=EDGE_LOOP('',(#10828,#10829,#10830,#10831));
#2633=EDGE_LOOP('',(#10832));
#2634=EDGE_LOOP('',(#10833));
#2635=EDGE_LOOP('',(#10834));
#2636=EDGE_LOOP('',(#10835));
#2637=EDGE_LOOP('',(#10836,#10837,#10838,#10839));
#2638=EDGE_LOOP('',(#10840,#10841,#10842,#10843));
#2639=EDGE_LOOP('',(#10844,#10845,#10846,#10847));
#2640=EDGE_LOOP('',(#10848,#10849,#10850,#10851));
#2641=EDGE_LOOP('',(#10852,#10853,#10854,#10855));
#2642=EDGE_LOOP('',(#10856,#10857,#10858,#10859));
#2643=EDGE_LOOP('',(#10860,#10861,#10862,#10863));
#2644=EDGE_LOOP('',(#10864,#10865,#10866,#10867));
#2645=EDGE_LOOP('',(#10868,#10869,#10870,#10871));
#2646=EDGE_LOOP('',(#10872,#10873,#10874,#10875));
#2647=EDGE_LOOP('',(#10876,#10877,#10878,#10879));
#2648=EDGE_LOOP('',(#10880,#10881,#10882,#10883));
#2649=EDGE_LOOP('',(#10884,#10885,#10886,#10887));
#2650=EDGE_LOOP('',(#10888,#10889,#10890,#10891));
#2651=EDGE_LOOP('',(#10892,#10893,#10894,#10895));
#2652=EDGE_LOOP('',(#10896,#10897,#10898,#10899));
#2653=EDGE_LOOP('',(#10900));
#2654=EDGE_LOOP('',(#10901,#10902,#10903,#10904));
#2655=EDGE_LOOP('',(#10905,#10906,#10907,#10908));
#2656=EDGE_LOOP('',(#10909,#10910,#10911,#10912));
#2657=EDGE_LOOP('',(#10913,#10914,#10915,#10916));
#2658=EDGE_LOOP('',(#10917,#10918,#10919,#10920));
#2659=EDGE_LOOP('',(#10921));
#2660=EDGE_LOOP('',(#10922,#10923,#10924,#10925));
#2661=EDGE_LOOP('',(#10926,#10927,#10928,#10929));
#2662=EDGE_LOOP('',(#10930));
#2663=EDGE_LOOP('',(#10931,#10932,#10933,#10934));
#2664=EDGE_LOOP('',(#10935,#10936,#10937,#10938));
#2665=EDGE_LOOP('',(#10939));
#2666=EDGE_LOOP('',(#10940,#10941,#10942,#10943));
#2667=EDGE_LOOP('',(#10944,#10945,#10946,#10947));
#2668=EDGE_LOOP('',(#10948,#10949,#10950,#10951));
#2669=EDGE_LOOP('',(#10952));
#2670=EDGE_LOOP('',(#10953));
#2671=EDGE_LOOP('',(#10954));
#2672=EDGE_LOOP('',(#10955));
#2673=EDGE_LOOP('',(#10956,#10957,#10958,#10959));
#2674=EDGE_LOOP('',(#10960,#10961,#10962,#10963));
#2675=EDGE_LOOP('',(#10964));
#2676=EDGE_LOOP('',(#10965));
#2677=EDGE_LOOP('',(#10966));
#2678=EDGE_LOOP('',(#10967));
#2679=EDGE_LOOP('',(#10968,#10969,#10970,#10971));
#2680=EDGE_LOOP('',(#10972,#10973,#10974,#10975));
#2681=EDGE_LOOP('',(#10976));
#2682=EDGE_LOOP('',(#10977));
#2683=EDGE_LOOP('',(#10978));
#2684=EDGE_LOOP('',(#10979));
#2685=EDGE_LOOP('',(#10980,#10981,#10982,#10983));
#2686=EDGE_LOOP('',(#10984,#10985,#10986,#10987));
#2687=EDGE_LOOP('',(#10988,#10989,#10990,#10991));
#2688=EDGE_LOOP('',(#10992,#10993,#10994,#10995,#10996,#10997,#10998,#10999,
#11000,#11001,#11002,#11003,#11004,#11005,#11006,#11007,#11008,#11009,#11010,
#11011,#11012,#11013,#11014,#11015,#11016,#11017,#11018,#11019,#11020,#11021,
#11022,#11023,#11024,#11025,#11026,#11027,#11028,#11029,#11030,#11031,#11032,
#11033,#11034,#11035,#11036,#11037,#11038,#11039,#11040,#11041,#11042,#11043,
#11044,#11045,#11046,#11047,#11048,#11049,#11050,#11051,#11052,#11053,#11054,
#11055,#11056,#11057,#11058,#11059,#11060,#11061,#11062,#11063,#11064,#11065,
#11066,#11067,#11068,#11069,#11070,#11071));
#2689=EDGE_LOOP('',(#11072,#11073,#11074,#11075));
#2690=EDGE_LOOP('',(#11076,#11077,#11078,#11079));
#2691=EDGE_LOOP('',(#11080,#11081,#11082,#11083));
#2692=EDGE_LOOP('',(#11084));
#2693=EDGE_LOOP('',(#11085,#11086,#11087,#11088));
#2694=EDGE_LOOP('',(#11089,#11090,#11091,#11092));
#2695=EDGE_LOOP('',(#11093,#11094,#11095,#11096));
#2696=EDGE_LOOP('',(#11097,#11098,#11099,#11100));
#2697=EDGE_LOOP('',(#11101,#11102,#11103,#11104));
#2698=EDGE_LOOP('',(#11105,#11106,#11107,#11108));
#2699=EDGE_LOOP('',(#11109,#11110,#11111,#11112));
#2700=EDGE_LOOP('',(#11113,#11114,#11115,#11116));
#2701=EDGE_LOOP('',(#11117,#11118,#11119,#11120));
#2702=EDGE_LOOP('',(#11121,#11122,#11123,#11124));
#2703=EDGE_LOOP('',(#11125,#11126,#11127,#11128));
#2704=EDGE_LOOP('',(#11129,#11130,#11131,#11132));
#2705=EDGE_LOOP('',(#11133,#11134,#11135,#11136));
#2706=EDGE_LOOP('',(#11137,#11138,#11139,#11140));
#2707=EDGE_LOOP('',(#11141,#11142,#11143,#11144));
#2708=EDGE_LOOP('',(#11145,#11146,#11147,#11148));
#2709=EDGE_LOOP('',(#11149,#11150,#11151,#11152));
#2710=EDGE_LOOP('',(#11153,#11154,#11155,#11156));
#2711=EDGE_LOOP('',(#11157,#11158,#11159,#11160));
#2712=EDGE_LOOP('',(#11161,#11162,#11163,#11164));
#2713=EDGE_LOOP('',(#11165,#11166,#11167,#11168));
#2714=EDGE_LOOP('',(#11169,#11170,#11171,#11172));
#2715=EDGE_LOOP('',(#11173,#11174,#11175,#11176));
#2716=EDGE_LOOP('',(#11177,#11178,#11179,#11180));
#2717=EDGE_LOOP('',(#11181,#11182,#11183,#11184));
#2718=EDGE_LOOP('',(#11185,#11186,#11187,#11188));
#2719=EDGE_LOOP('',(#11189,#11190,#11191,#11192));
#2720=EDGE_LOOP('',(#11193,#11194,#11195,#11196));
#2721=EDGE_LOOP('',(#11197,#11198,#11199,#11200));
#2722=EDGE_LOOP('',(#11201,#11202,#11203,#11204));
#2723=EDGE_LOOP('',(#11205,#11206,#11207,#11208));
#2724=EDGE_LOOP('',(#11209,#11210,#11211,#11212));
#2725=EDGE_LOOP('',(#11213,#11214,#11215,#11216));
#2726=EDGE_LOOP('',(#11217,#11218,#11219,#11220));
#2727=EDGE_LOOP('',(#11221,#11222,#11223,#11224));
#2728=EDGE_LOOP('',(#11225,#11226,#11227,#11228));
#2729=EDGE_LOOP('',(#11229,#11230,#11231,#11232));
#2730=EDGE_LOOP('',(#11233,#11234,#11235,#11236));
#2731=EDGE_LOOP('',(#11237,#11238,#11239,#11240));
#2732=EDGE_LOOP('',(#11241,#11242,#11243,#11244));
#2733=EDGE_LOOP('',(#11245,#11246,#11247,#11248));
#2734=EDGE_LOOP('',(#11249,#11250,#11251,#11252));
#2735=EDGE_LOOP('',(#11253,#11254,#11255,#11256));
#2736=EDGE_LOOP('',(#11257,#11258,#11259,#11260));
#2737=EDGE_LOOP('',(#11261,#11262,#11263,#11264));
#2738=EDGE_LOOP('',(#11265,#11266,#11267,#11268));
#2739=EDGE_LOOP('',(#11269,#11270,#11271,#11272));
#2740=EDGE_LOOP('',(#11273,#11274,#11275,#11276));
#2741=EDGE_LOOP('',(#11277,#11278,#11279,#11280));
#2742=EDGE_LOOP('',(#11281,#11282,#11283,#11284));
#2743=EDGE_LOOP('',(#11285,#11286,#11287,#11288));
#2744=EDGE_LOOP('',(#11289,#11290,#11291,#11292));
#2745=EDGE_LOOP('',(#11293,#11294,#11295,#11296));
#2746=EDGE_LOOP('',(#11297,#11298,#11299,#11300));
#2747=EDGE_LOOP('',(#11301,#11302,#11303,#11304));
#2748=EDGE_LOOP('',(#11305,#11306,#11307,#11308));
#2749=EDGE_LOOP('',(#11309,#11310,#11311,#11312));
#2750=EDGE_LOOP('',(#11313,#11314,#11315,#11316));
#2751=EDGE_LOOP('',(#11317,#11318,#11319,#11320));
#2752=EDGE_LOOP('',(#11321,#11322,#11323,#11324));
#2753=EDGE_LOOP('',(#11325,#11326,#11327,#11328));
#2754=EDGE_LOOP('',(#11329,#11330,#11331,#11332));
#2755=EDGE_LOOP('',(#11333,#11334,#11335,#11336));
#2756=EDGE_LOOP('',(#11337,#11338,#11339,#11340));
#2757=EDGE_LOOP('',(#11341,#11342,#11343,#11344));
#2758=EDGE_LOOP('',(#11345,#11346,#11347,#11348));
#2759=EDGE_LOOP('',(#11349,#11350,#11351,#11352));
#2760=EDGE_LOOP('',(#11353,#11354,#11355,#11356));
#2761=EDGE_LOOP('',(#11357,#11358,#11359,#11360));
#2762=EDGE_LOOP('',(#11361,#11362,#11363,#11364));
#2763=EDGE_LOOP('',(#11365,#11366,#11367,#11368));
#2764=EDGE_LOOP('',(#11369,#11370,#11371,#11372));
#2765=EDGE_LOOP('',(#11373,#11374,#11375,#11376));
#2766=EDGE_LOOP('',(#11377,#11378,#11379,#11380));
#2767=EDGE_LOOP('',(#11381,#11382,#11383,#11384));
#2768=EDGE_LOOP('',(#11385,#11386,#11387,#11388));
#2769=EDGE_LOOP('',(#11389,#11390,#11391,#11392));
#2770=EDGE_LOOP('',(#11393,#11394,#11395,#11396));
#2771=EDGE_LOOP('',(#11397,#11398,#11399,#11400));
#2772=EDGE_LOOP('',(#11401,#11402,#11403,#11404));
#2773=EDGE_LOOP('',(#11405,#11406,#11407,#11408,#11409,#11410,#11411,#11412,
#11413,#11414,#11415,#11416,#11417,#11418,#11419,#11420,#11421,#11422,#11423,
#11424,#11425,#11426,#11427,#11428,#11429,#11430,#11431,#11432,#11433,#11434,
#11435,#11436,#11437,#11438,#11439,#11440,#11441,#11442,#11443,#11444,#11445,
#11446,#11447,#11448,#11449,#11450,#11451,#11452,#11453,#11454,#11455,#11456,
#11457,#11458,#11459,#11460,#11461,#11462,#11463,#11464,#11465,#11466,#11467,
#11468,#11469,#11470,#11471,#11472,#11473,#11474,#11475,#11476,#11477,#11478,
#11479,#11480,#11481,#11482,#11483,#11484));
#2774=EDGE_LOOP('',(#11485));
#2775=EDGE_LOOP('',(#11486,#11487,#11488,#11489));
#2776=EDGE_LOOP('',(#11490,#11491,#11492,#11493));
#2777=EDGE_LOOP('',(#11494,#11495,#11496,#11497));
#2778=EDGE_LOOP('',(#11498));
#2779=EDGE_LOOP('',(#11499));
#2780=EDGE_LOOP('',(#11500));
#2781=EDGE_LOOP('',(#11501));
#2782=EDGE_LOOP('',(#11502));
#2783=EDGE_LOOP('',(#11503,#11504,#11505,#11506));
#2784=EDGE_LOOP('',(#11507,#11508,#11509,#11510));
#2785=EDGE_LOOP('',(#11511,#11512,#11513,#11514));
#2786=EDGE_LOOP('',(#11515));
#2787=EDGE_LOOP('',(#11516));
#2788=EDGE_LOOP('',(#11517,#11518,#11519,#11520));
#2789=EDGE_LOOP('',(#11521,#11522,#11523,#11524));
#2790=EDGE_LOOP('',(#11525,#11526,#11527,#11528));
#2791=EDGE_LOOP('',(#11529));
#2792=EDGE_LOOP('',(#11530,#11531,#11532,#11533));
#2793=EDGE_LOOP('',(#11534,#11535,#11536,#11537));
#2794=EDGE_LOOP('',(#11538,#11539,#11540,#11541));
#2795=EDGE_LOOP('',(#11542,#11543,#11544,#11545));
#2796=EDGE_LOOP('',(#11546,#11547,#11548,#11549));
#2797=EDGE_LOOP('',(#11550,#11551,#11552,#11553));
#2798=EDGE_LOOP('',(#11554,#11555,#11556,#11557,#11558,#11559));
#2799=EDGE_LOOP('',(#11560,#11561,#11562,#11563,#11564,#11565));
#2800=EDGE_LOOP('',(#11566));
#2801=EDGE_LOOP('',(#11567,#11568,#11569,#11570));
#2802=EDGE_LOOP('',(#11571,#11572,#11573,#11574));
#2803=EDGE_LOOP('',(#11575,#11576,#11577,#11578));
#2804=EDGE_LOOP('',(#11579));
#2805=EDGE_LOOP('',(#11580));
#2806=EDGE_LOOP('',(#11581,#11582,#11583,#11584));
#2807=EDGE_LOOP('',(#11585,#11586,#11587,#11588));
#2808=EDGE_LOOP('',(#11589,#11590,#11591,#11592));
#2809=EDGE_LOOP('',(#11593));
#2810=EDGE_LOOP('',(#11594,#11595,#11596,#11597));
#2811=EDGE_LOOP('',(#11598,#11599,#11600,#11601));
#2812=EDGE_LOOP('',(#11602,#11603,#11604,#11605));
#2813=EDGE_LOOP('',(#11606,#11607,#11608,#11609));
#2814=EDGE_LOOP('',(#11610,#11611,#11612,#11613));
#2815=EDGE_LOOP('',(#11614,#11615,#11616,#11617));
#2816=EDGE_LOOP('',(#11618,#11619,#11620,#11621,#11622,#11623));
#2817=EDGE_LOOP('',(#11624,#11625,#11626,#11627,#11628,#11629));
#2818=EDGE_LOOP('',(#11630,#11631,#11632,#11633));
#2819=EDGE_LOOP('',(#11634,#11635,#11636,#11637));
#2820=EDGE_LOOP('',(#11638));
#2821=EDGE_LOOP('',(#11639));
#2822=EDGE_LOOP('',(#11640));
#2823=EDGE_LOOP('',(#11641));
#2824=LINE('',#17645,#3995);
#2825=LINE('',#17651,#3996);
#2826=LINE('',#17657,#3997);
#2827=LINE('',#17663,#3998);
#2828=LINE('',#17669,#3999);
#2829=LINE('',#17675,#4000);
#2830=LINE('',#17681,#4001);
#2831=LINE('',#17687,#4002);
#2832=LINE('',#17693,#4003);
#2833=LINE('',#17699,#4004);
#2834=LINE('',#17704,#4005);
#2835=LINE('',#17706,#4006);
#2836=LINE('',#17708,#4007);
#2837=LINE('',#17709,#4008);
#2838=LINE('',#17712,#4009);
#2839=LINE('',#17714,#4010);
#2840=LINE('',#17715,#4011);
#2841=LINE('',#17718,#4012);
#2842=LINE('',#17720,#4013);
#2843=LINE('',#17721,#4014);
#2844=LINE('',#17723,#4015);
#2845=LINE('',#17724,#4016);
#2846=LINE('',#17731,#4017);
#2847=LINE('',#17733,#4018);
#2848=LINE('',#17735,#4019);
#2849=LINE('',#17736,#4020);
#2850=LINE('',#17739,#4021);
#2851=LINE('',#17741,#4022);
#2852=LINE('',#17742,#4023);
#2853=LINE('',#17745,#4024);
#2854=LINE('',#17747,#4025);
#2855=LINE('',#17748,#4026);
#2856=LINE('',#17750,#4027);
#2857=LINE('',#17751,#4028);
#2858=LINE('',#17758,#4029);
#2859=LINE('',#17760,#4030);
#2860=LINE('',#17762,#4031);
#2861=LINE('',#17763,#4032);
#2862=LINE('',#17766,#4033);
#2863=LINE('',#17768,#4034);
#2864=LINE('',#17769,#4035);
#2865=LINE('',#17772,#4036);
#2866=LINE('',#17774,#4037);
#2867=LINE('',#17775,#4038);
#2868=LINE('',#17777,#4039);
#2869=LINE('',#17778,#4040);
#2870=LINE('',#17786,#4041);
#2871=LINE('',#17793,#4042);
#2872=LINE('',#17799,#4043);
#2873=LINE('',#17801,#4044);
#2874=LINE('',#17803,#4045);
#2875=LINE('',#17804,#4046);
#2876=LINE('',#17808,#4047);
#2877=LINE('',#17810,#4048);
#2878=LINE('',#17812,#4049);
#2879=LINE('',#17813,#4050);
#2880=LINE('',#17818,#4051);
#2881=LINE('',#17820,#4052);
#2882=LINE('',#17822,#4053);
#2883=LINE('',#17829,#4054);
#2884=LINE('',#17834,#4055);
#2885=LINE('',#17837,#4056);
#2886=LINE('',#17839,#4057);
#2887=LINE('',#17840,#4058);
#2888=LINE('',#17842,#4059);
#2889=LINE('',#17844,#4060);
#2890=LINE('',#17849,#4061);
#2891=LINE('',#17856,#4062);
#2892=LINE('',#17862,#4063);
#2893=LINE('',#17864,#4064);
#2894=LINE('',#17866,#4065);
#2895=LINE('',#17867,#4066);
#2896=LINE('',#17871,#4067);
#2897=LINE('',#17873,#4068);
#2898=LINE('',#17875,#4069);
#2899=LINE('',#17876,#4070);
#2900=LINE('',#17881,#4071);
#2901=LINE('',#17883,#4072);
#2902=LINE('',#17885,#4073);
#2903=LINE('',#17892,#4074);
#2904=LINE('',#17897,#4075);
#2905=LINE('',#17900,#4076);
#2906=LINE('',#17902,#4077);
#2907=LINE('',#17903,#4078);
#2908=LINE('',#17905,#4079);
#2909=LINE('',#17907,#4080);
#2910=LINE('',#17912,#4081);
#2911=LINE('',#17918,#4082);
#2912=LINE('',#17924,#4083);
#2913=LINE('',#17930,#4084);
#2914=LINE('',#17935,#4085);
#2915=LINE('',#17937,#4086);
#2916=LINE('',#17939,#4087);
#2917=LINE('',#17940,#4088);
#2918=LINE('',#17943,#4089);
#2919=LINE('',#17945,#4090);
#2920=LINE('',#17947,#4091);
#2921=LINE('',#17948,#4092);
#2922=LINE('',#17952,#4093);
#2923=LINE('',#17953,#4094);
#2924=LINE('',#17954,#4095);
#2925=LINE('',#17957,#4096);
#2926=LINE('',#17958,#4097);
#2927=LINE('',#17961,#4098);
#2928=LINE('',#17962,#4099);
#2929=LINE('',#17964,#4100);
#2930=LINE('',#17967,#4101);
#2931=LINE('',#17969,#4102);
#2932=LINE('',#17970,#4103);
#2933=LINE('',#17973,#4104);
#2934=LINE('',#17974,#4105);
#2935=LINE('',#17977,#4106);
#2936=LINE('',#17978,#4107);
#2937=LINE('',#17980,#4108);
#2938=LINE('',#17987,#4109);
#2939=LINE('',#17989,#4110);
#2940=LINE('',#17991,#4111);
#2941=LINE('',#17992,#4112);
#2942=LINE('',#17996,#4113);
#2943=LINE('',#17998,#4114);
#2944=LINE('',#18000,#4115);
#2945=LINE('',#18001,#4116);
#2946=LINE('',#18004,#4117);
#2947=LINE('',#18006,#4118);
#2948=LINE('',#18008,#4119);
#2949=LINE('',#18010,#4120);
#2950=LINE('',#18011,#4121);
#2951=LINE('',#18014,#4122);
#2952=LINE('',#18016,#4123);
#2953=LINE('',#18018,#4124);
#2954=LINE('',#18020,#4125);
#2955=LINE('',#18021,#4126);
#2956=LINE('',#18039,#4127);
#2957=LINE('',#18045,#4128);
#2958=LINE('',#18050,#4129);
#2959=LINE('',#18052,#4130);
#2960=LINE('',#18054,#4131);
#2961=LINE('',#18055,#4132);
#2962=LINE('',#18059,#4133);
#2963=LINE('',#18061,#4134);
#2964=LINE('',#18063,#4135);
#2965=LINE('',#18064,#4136);
#2966=LINE('',#18067,#4137);
#2967=LINE('',#18069,#4138);
#2968=LINE('',#18070,#4139);
#2969=LINE('',#18073,#4140);
#2970=LINE('',#18075,#4141);
#2971=LINE('',#18076,#4142);
#2972=LINE('',#18079,#4143);
#2973=LINE('',#18081,#4144);
#2974=LINE('',#18082,#4145);
#2975=LINE('',#18085,#4146);
#2976=LINE('',#18087,#4147);
#2977=LINE('',#18088,#4148);
#2978=LINE('',#18092,#4149);
#2979=LINE('',#18094,#4150);
#2980=LINE('',#18095,#4151);
#2981=LINE('',#18100,#4152);
#2982=LINE('',#18101,#4153);
#2983=LINE('',#18104,#4154);
#2984=LINE('',#18105,#4155);
#2985=LINE('',#18107,#4156);
#2986=LINE('',#18113,#4157);
#2987=LINE('',#18115,#4158);
#2988=LINE('',#18117,#4159);
#2989=LINE('',#18118,#4160);
#2990=LINE('',#18122,#4161);
#2991=LINE('',#18124,#4162);
#2992=LINE('',#18126,#4163);
#2993=LINE('',#18127,#4164);
#2994=LINE('',#18130,#4165);
#2995=LINE('',#18132,#4166);
#2996=LINE('',#18134,#4167);
#2997=LINE('',#18136,#4168);
#2998=LINE('',#18137,#4169);
#2999=LINE('',#18140,#4170);
#3000=LINE('',#18142,#4171);
#3001=LINE('',#18144,#4172);
#3002=LINE('',#18146,#4173);
#3003=LINE('',#18147,#4174);
#3004=LINE('',#18165,#4175);
#3005=LINE('',#18171,#4176);
#3006=LINE('',#18176,#4177);
#3007=LINE('',#18178,#4178);
#3008=LINE('',#18180,#4179);
#3009=LINE('',#18181,#4180);
#3010=LINE('',#18185,#4181);
#3011=LINE('',#18187,#4182);
#3012=LINE('',#18189,#4183);
#3013=LINE('',#18190,#4184);
#3014=LINE('',#18193,#4185);
#3015=LINE('',#18195,#4186);
#3016=LINE('',#18196,#4187);
#3017=LINE('',#18199,#4188);
#3018=LINE('',#18201,#4189);
#3019=LINE('',#18202,#4190);
#3020=LINE('',#18205,#4191);
#3021=LINE('',#18207,#4192);
#3022=LINE('',#18208,#4193);
#3023=LINE('',#18211,#4194);
#3024=LINE('',#18213,#4195);
#3025=LINE('',#18214,#4196);
#3026=LINE('',#18218,#4197);
#3027=LINE('',#18220,#4198);
#3028=LINE('',#18221,#4199);
#3029=LINE('',#18226,#4200);
#3030=LINE('',#18227,#4201);
#3031=LINE('',#18230,#4202);
#3032=LINE('',#18231,#4203);
#3033=LINE('',#18233,#4204);
#3034=LINE('',#18240,#4205);
#3035=LINE('',#18249,#4206);
#3036=LINE('',#18257,#4207);
#3037=LINE('',#18261,#4208);
#3038=LINE('',#18266,#4209);
#3039=LINE('',#18276,#4210);
#3040=LINE('',#18279,#4211);
#3041=LINE('',#18282,#4212);
#3042=LINE('',#18284,#4213);
#3043=LINE('',#18286,#4214);
#3044=LINE('',#18287,#4215);
#3045=LINE('',#18294,#4216);
#3046=LINE('',#18295,#4217);
#3047=LINE('',#18300,#4218);
#3048=LINE('',#18306,#4219);
#3049=LINE('',#18312,#4220);
#3050=LINE('',#18318,#4221);
#3051=LINE('',#18322,#4222);
#3052=LINE('',#18326,#4223);
#3053=LINE('',#18332,#4224);
#3054=LINE('',#18336,#4225);
#3055=LINE('',#18338,#4226);
#3056=LINE('',#18339,#4227);
#3057=LINE('',#18343,#4228);
#3058=LINE('',#18345,#4229);
#3059=LINE('',#18347,#4230);
#3060=LINE('',#18348,#4231);
#3061=LINE('',#18350,#4232);
#3062=LINE('',#18351,#4233);
#3063=LINE('',#18354,#4234);
#3064=LINE('',#18356,#4235);
#3065=LINE('',#18357,#4236);
#3066=LINE('',#18360,#4237);
#3067=LINE('',#18361,#4238);
#3068=LINE('',#18364,#4239);
#3069=LINE('',#18365,#4240);
#3070=LINE('',#18367,#4241);
#3071=LINE('',#18374,#4242);
#3072=LINE('',#18380,#4243);
#3073=LINE('',#18386,#4244);
#3074=LINE('',#18392,#4245);
#3075=LINE('',#18398,#4246);
#3076=LINE('',#18404,#4247);
#3077=LINE('',#18411,#4248);
#3078=LINE('',#18420,#4249);
#3079=LINE('',#18426,#4250);
#3080=LINE('',#18432,#4251);
#3081=LINE('',#18438,#4252);
#3082=LINE('',#18444,#4253);
#3083=LINE('',#18450,#4254);
#3084=LINE('',#18457,#4255);
#3085=LINE('',#18467,#4256);
#3086=LINE('',#18470,#4257);
#3087=LINE('',#18473,#4258);
#3088=LINE('',#18475,#4259);
#3089=LINE('',#18477,#4260);
#3090=LINE('',#18478,#4261);
#3091=LINE('',#18485,#4262);
#3092=LINE('',#18487,#4263);
#3093=LINE('',#18489,#4264);
#3094=LINE('',#18491,#4265);
#3095=LINE('',#18493,#4266);
#3096=LINE('',#18494,#4267);
#3097=LINE('',#18507,#4268);
#3098=LINE('',#18511,#4269);
#3099=LINE('',#18515,#4270);
#3100=LINE('',#18519,#4271);
#3101=LINE('',#18523,#4272);
#3102=LINE('',#18527,#4273);
#3103=LINE('',#18531,#4274);
#3104=LINE('',#18535,#4275);
#3105=LINE('',#18537,#4276);
#3106=LINE('',#18538,#4277);
#3107=LINE('',#18541,#4278);
#3108=LINE('',#18543,#4279);
#3109=LINE('',#18544,#4280);
#3110=LINE('',#18546,#4281);
#3111=LINE('',#18548,#4282);
#3112=LINE('',#18551,#4283);
#3113=LINE('',#18552,#4284);
#3114=LINE('',#18555,#4285);
#3115=LINE('',#18556,#4286);
#3116=LINE('',#18558,#4287);
#3117=LINE('',#18565,#4288);
#3118=LINE('',#18571,#4289);
#3119=LINE('',#18577,#4290);
#3120=LINE('',#18583,#4291);
#3121=LINE('',#18589,#4292);
#3122=LINE('',#18595,#4293);
#3123=LINE('',#18602,#4294);
#3124=LINE('',#18611,#4295);
#3125=LINE('',#18617,#4296);
#3126=LINE('',#18623,#4297);
#3127=LINE('',#18629,#4298);
#3128=LINE('',#18635,#4299);
#3129=LINE('',#18641,#4300);
#3130=LINE('',#18648,#4301);
#3131=LINE('',#18659,#4302);
#3132=LINE('',#18663,#4303);
#3133=LINE('',#18667,#4304);
#3134=LINE('',#18674,#4305);
#3135=LINE('',#18678,#4306);
#3136=LINE('',#18682,#4307);
#3137=LINE('',#18687,#4308);
#3138=LINE('',#18689,#4309);
#3139=LINE('',#18691,#4310);
#3140=LINE('',#18692,#4311);
#3141=LINE('',#18695,#4312);
#3142=LINE('',#18697,#4313);
#3143=LINE('',#18698,#4314);
#3144=LINE('',#18701,#4315);
#3145=LINE('',#18703,#4316);
#3146=LINE('',#18704,#4317);
#3147=LINE('',#18707,#4318);
#3148=LINE('',#18709,#4319);
#3149=LINE('',#18710,#4320);
#3150=LINE('',#18713,#4321);
#3151=LINE('',#18715,#4322);
#3152=LINE('',#18716,#4323);
#3153=LINE('',#18718,#4324);
#3154=LINE('',#18719,#4325);
#3155=LINE('',#18736,#4326);
#3156=LINE('',#18742,#4327);
#3157=LINE('',#18746,#4328);
#3158=LINE('',#18752,#4329);
#3159=LINE('',#18757,#4330);
#3160=LINE('',#18772,#4331);
#3161=LINE('',#18781,#4332);
#3162=LINE('',#18785,#4333);
#3163=LINE('',#18789,#4334);
#3164=LINE('',#18792,#4335);
#3165=LINE('',#18928,#4336);
#3166=LINE('',#19181,#4337);
#3167=LINE('',#19223,#4338);
#3168=LINE('',#19228,#4339);
#3169=LINE('',#19237,#4340);
#3170=LINE('',#19242,#4341);
#3171=LINE('',#19252,#4342);
#3172=LINE('',#19254,#4343);
#3173=LINE('',#19256,#4344);
#3174=LINE('',#19257,#4345);
#3175=LINE('',#19260,#4346);
#3176=LINE('',#19262,#4347);
#3177=LINE('',#19263,#4348);
#3178=LINE('',#19266,#4349);
#3179=LINE('',#19268,#4350);
#3180=LINE('',#19269,#4351);
#3181=LINE('',#19272,#4352);
#3182=LINE('',#19274,#4353);
#3183=LINE('',#19275,#4354);
#3184=LINE('',#19278,#4355);
#3185=LINE('',#19280,#4356);
#3186=LINE('',#19281,#4357);
#3187=LINE('',#19283,#4358);
#3188=LINE('',#19284,#4359);
#3189=LINE('',#19296,#4360);
#3190=LINE('',#19300,#4361);
#3191=LINE('',#19304,#4362);
#3192=LINE('',#19311,#4363);
#3193=LINE('',#19313,#4364);
#3194=LINE('',#19320,#4365);
#3195=LINE('',#19326,#4366);
#3196=LINE('',#19328,#4367);
#3197=LINE('',#19330,#4368);
#3198=LINE('',#19331,#4369);
#3199=LINE('',#19335,#4370);
#3200=LINE('',#19337,#4371);
#3201=LINE('',#19339,#4372);
#3202=LINE('',#19340,#4373);
#3203=LINE('',#19345,#4374);
#3204=LINE('',#19347,#4375);
#3205=LINE('',#19348,#4376);
#3206=LINE('',#19354,#4377);
#3207=LINE('',#19356,#4378);
#3208=LINE('',#19357,#4379);
#3209=LINE('',#19361,#4380);
#3210=LINE('',#19363,#4381);
#3211=LINE('',#19364,#4382);
#3212=LINE('',#19367,#4383);
#3213=LINE('',#19369,#4384);
#3214=LINE('',#19370,#4385);
#3215=LINE('',#19373,#4386);
#3216=LINE('',#19375,#4387);
#3217=LINE('',#19376,#4388);
#3218=LINE('',#19379,#4389);
#3219=LINE('',#19381,#4390);
#3220=LINE('',#19382,#4391);
#3221=LINE('',#19385,#4392);
#3222=LINE('',#19387,#4393);
#3223=LINE('',#19388,#4394);
#3224=LINE('',#19391,#4395);
#3225=LINE('',#19393,#4396);
#3226=LINE('',#19394,#4397);
#3227=LINE('',#19397,#4398);
#3228=LINE('',#19399,#4399);
#3229=LINE('',#19400,#4400);
#3230=LINE('',#19403,#4401);
#3231=LINE('',#19405,#4402);
#3232=LINE('',#19406,#4403);
#3233=LINE('',#19409,#4404);
#3234=LINE('',#19411,#4405);
#3235=LINE('',#19412,#4406);
#3236=LINE('',#19415,#4407);
#3237=LINE('',#19417,#4408);
#3238=LINE('',#19418,#4409);
#3239=LINE('',#19421,#4410);
#3240=LINE('',#19423,#4411);
#3241=LINE('',#19424,#4412);
#3242=LINE('',#19427,#4413);
#3243=LINE('',#19429,#4414);
#3244=LINE('',#19430,#4415);
#3245=LINE('',#19433,#4416);
#3246=LINE('',#19435,#4417);
#3247=LINE('',#19436,#4418);
#3248=LINE('',#19439,#4419);
#3249=LINE('',#19441,#4420);
#3250=LINE('',#19442,#4421);
#3251=LINE('',#19445,#4422);
#3252=LINE('',#19447,#4423);
#3253=LINE('',#19448,#4424);
#3254=LINE('',#19451,#4425);
#3255=LINE('',#19453,#4426);
#3256=LINE('',#19454,#4427);
#3257=LINE('',#19457,#4428);
#3258=LINE('',#19459,#4429);
#3259=LINE('',#19460,#4430);
#3260=LINE('',#19463,#4431);
#3261=LINE('',#19465,#4432);
#3262=LINE('',#19466,#4433);
#3263=LINE('',#19469,#4434);
#3264=LINE('',#19471,#4435);
#3265=LINE('',#19472,#4436);
#3266=LINE('',#19475,#4437);
#3267=LINE('',#19477,#4438);
#3268=LINE('',#19478,#4439);
#3269=LINE('',#19481,#4440);
#3270=LINE('',#19483,#4441);
#3271=LINE('',#19484,#4442);
#3272=LINE('',#19487,#4443);
#3273=LINE('',#19489,#4444);
#3274=LINE('',#19490,#4445);
#3275=LINE('',#19493,#4446);
#3276=LINE('',#19495,#4447);
#3277=LINE('',#19496,#4448);
#3278=LINE('',#19499,#4449);
#3279=LINE('',#19501,#4450);
#3280=LINE('',#19502,#4451);
#3281=LINE('',#19505,#4452);
#3282=LINE('',#19507,#4453);
#3283=LINE('',#19508,#4454);
#3284=LINE('',#19511,#4455);
#3285=LINE('',#19513,#4456);
#3286=LINE('',#19514,#4457);
#3287=LINE('',#19517,#4458);
#3288=LINE('',#19519,#4459);
#3289=LINE('',#19520,#4460);
#3290=LINE('',#19523,#4461);
#3291=LINE('',#19525,#4462);
#3292=LINE('',#19526,#4463);
#3293=LINE('',#19529,#4464);
#3294=LINE('',#19531,#4465);
#3295=LINE('',#19532,#4466);
#3296=LINE('',#19535,#4467);
#3297=LINE('',#19537,#4468);
#3298=LINE('',#19538,#4469);
#3299=LINE('',#19541,#4470);
#3300=LINE('',#19543,#4471);
#3301=LINE('',#19544,#4472);
#3302=LINE('',#19547,#4473);
#3303=LINE('',#19549,#4474);
#3304=LINE('',#19550,#4475);
#3305=LINE('',#19553,#4476);
#3306=LINE('',#19555,#4477);
#3307=LINE('',#19556,#4478);
#3308=LINE('',#19559,#4479);
#3309=LINE('',#19561,#4480);
#3310=LINE('',#19562,#4481);
#3311=LINE('',#19565,#4482);
#3312=LINE('',#19567,#4483);
#3313=LINE('',#19568,#4484);
#3314=LINE('',#19571,#4485);
#3315=LINE('',#19573,#4486);
#3316=LINE('',#19574,#4487);
#3317=LINE('',#19577,#4488);
#3318=LINE('',#19579,#4489);
#3319=LINE('',#19580,#4490);
#3320=LINE('',#19583,#4491);
#3321=LINE('',#19585,#4492);
#3322=LINE('',#19586,#4493);
#3323=LINE('',#19589,#4494);
#3324=LINE('',#19591,#4495);
#3325=LINE('',#19592,#4496);
#3326=LINE('',#19595,#4497);
#3327=LINE('',#19597,#4498);
#3328=LINE('',#19598,#4499);
#3329=LINE('',#19601,#4500);
#3330=LINE('',#19603,#4501);
#3331=LINE('',#19604,#4502);
#3332=LINE('',#19607,#4503);
#3333=LINE('',#19609,#4504);
#3334=LINE('',#19610,#4505);
#3335=LINE('',#19613,#4506);
#3336=LINE('',#19615,#4507);
#3337=LINE('',#19616,#4508);
#3338=LINE('',#19619,#4509);
#3339=LINE('',#19621,#4510);
#3340=LINE('',#19622,#4511);
#3341=LINE('',#19625,#4512);
#3342=LINE('',#19627,#4513);
#3343=LINE('',#19628,#4514);
#3344=LINE('',#19631,#4515);
#3345=LINE('',#19633,#4516);
#3346=LINE('',#19634,#4517);
#3347=LINE('',#19637,#4518);
#3348=LINE('',#19639,#4519);
#3349=LINE('',#19640,#4520);
#3350=LINE('',#19643,#4521);
#3351=LINE('',#19645,#4522);
#3352=LINE('',#19646,#4523);
#3353=LINE('',#19649,#4524);
#3354=LINE('',#19651,#4525);
#3355=LINE('',#19652,#4526);
#3356=LINE('',#19655,#4527);
#3357=LINE('',#19657,#4528);
#3358=LINE('',#19658,#4529);
#3359=LINE('',#19661,#4530);
#3360=LINE('',#19663,#4531);
#3361=LINE('',#19664,#4532);
#3362=LINE('',#19667,#4533);
#3363=LINE('',#19669,#4534);
#3364=LINE('',#19670,#4535);
#3365=LINE('',#19673,#4536);
#3366=LINE('',#19675,#4537);
#3367=LINE('',#19676,#4538);
#3368=LINE('',#19679,#4539);
#3369=LINE('',#19681,#4540);
#3370=LINE('',#19682,#4541);
#3371=LINE('',#19685,#4542);
#3372=LINE('',#19687,#4543);
#3373=LINE('',#19688,#4544);
#3374=LINE('',#19691,#4545);
#3375=LINE('',#19693,#4546);
#3376=LINE('',#19694,#4547);
#3377=LINE('',#19697,#4548);
#3378=LINE('',#19699,#4549);
#3379=LINE('',#19700,#4550);
#3380=LINE('',#19703,#4551);
#3381=LINE('',#19705,#4552);
#3382=LINE('',#19706,#4553);
#3383=LINE('',#19709,#4554);
#3384=LINE('',#19711,#4555);
#3385=LINE('',#19712,#4556);
#3386=LINE('',#19715,#4557);
#3387=LINE('',#19717,#4558);
#3388=LINE('',#19718,#4559);
#3389=LINE('',#19721,#4560);
#3390=LINE('',#19723,#4561);
#3391=LINE('',#19724,#4562);
#3392=LINE('',#19727,#4563);
#3393=LINE('',#19729,#4564);
#3394=LINE('',#19730,#4565);
#3395=LINE('',#19733,#4566);
#3396=LINE('',#19735,#4567);
#3397=LINE('',#19736,#4568);
#3398=LINE('',#19739,#4569);
#3399=LINE('',#19741,#4570);
#3400=LINE('',#19742,#4571);
#3401=LINE('',#19745,#4572);
#3402=LINE('',#19747,#4573);
#3403=LINE('',#19748,#4574);
#3404=LINE('',#19751,#4575);
#3405=LINE('',#19753,#4576);
#3406=LINE('',#19754,#4577);
#3407=LINE('',#19757,#4578);
#3408=LINE('',#19759,#4579);
#3409=LINE('',#19760,#4580);
#3410=LINE('',#19763,#4581);
#3411=LINE('',#19765,#4582);
#3412=LINE('',#19766,#4583);
#3413=LINE('',#19769,#4584);
#3414=LINE('',#19771,#4585);
#3415=LINE('',#19772,#4586);
#3416=LINE('',#19775,#4587);
#3417=LINE('',#19777,#4588);
#3418=LINE('',#19778,#4589);
#3419=LINE('',#19781,#4590);
#3420=LINE('',#19783,#4591);
#3421=LINE('',#19784,#4592);
#3422=LINE('',#19787,#4593);
#3423=LINE('',#19789,#4594);
#3424=LINE('',#19790,#4595);
#3425=LINE('',#19793,#4596);
#3426=LINE('',#19795,#4597);
#3427=LINE('',#19796,#4598);
#3428=LINE('',#19799,#4599);
#3429=LINE('',#19801,#4600);
#3430=LINE('',#19802,#4601);
#3431=LINE('',#19805,#4602);
#3432=LINE('',#19807,#4603);
#3433=LINE('',#19808,#4604);
#3434=LINE('',#19811,#4605);
#3435=LINE('',#19813,#4606);
#3436=LINE('',#19814,#4607);
#3437=LINE('',#19817,#4608);
#3438=LINE('',#19819,#4609);
#3439=LINE('',#19820,#4610);
#3440=LINE('',#19823,#4611);
#3441=LINE('',#19825,#4612);
#3442=LINE('',#19826,#4613);
#3443=LINE('',#19829,#4614);
#3444=LINE('',#19831,#4615);
#3445=LINE('',#19832,#4616);
#3446=LINE('',#19835,#4617);
#3447=LINE('',#19837,#4618);
#3448=LINE('',#19838,#4619);
#3449=LINE('',#19841,#4620);
#3450=LINE('',#19843,#4621);
#3451=LINE('',#19844,#4622);
#3452=LINE('',#19847,#4623);
#3453=LINE('',#19849,#4624);
#3454=LINE('',#19850,#4625);
#3455=LINE('',#19853,#4626);
#3456=LINE('',#19855,#4627);
#3457=LINE('',#19856,#4628);
#3458=LINE('',#19859,#4629);
#3459=LINE('',#19861,#4630);
#3460=LINE('',#19862,#4631);
#3461=LINE('',#19865,#4632);
#3462=LINE('',#19867,#4633);
#3463=LINE('',#19868,#4634);
#3464=LINE('',#19871,#4635);
#3465=LINE('',#19873,#4636);
#3466=LINE('',#19874,#4637);
#3467=LINE('',#19877,#4638);
#3468=LINE('',#19879,#4639);
#3469=LINE('',#19880,#4640);
#3470=LINE('',#19883,#4641);
#3471=LINE('',#19885,#4642);
#3472=LINE('',#19886,#4643);
#3473=LINE('',#19889,#4644);
#3474=LINE('',#19891,#4645);
#3475=LINE('',#19892,#4646);
#3476=LINE('',#19895,#4647);
#3477=LINE('',#19897,#4648);
#3478=LINE('',#19898,#4649);
#3479=LINE('',#19901,#4650);
#3480=LINE('',#19903,#4651);
#3481=LINE('',#19904,#4652);
#3482=LINE('',#19907,#4653);
#3483=LINE('',#19909,#4654);
#3484=LINE('',#19910,#4655);
#3485=LINE('',#19913,#4656);
#3486=LINE('',#19915,#4657);
#3487=LINE('',#19916,#4658);
#3488=LINE('',#19919,#4659);
#3489=LINE('',#19921,#4660);
#3490=LINE('',#19922,#4661);
#3491=LINE('',#19925,#4662);
#3492=LINE('',#19927,#4663);
#3493=LINE('',#19928,#4664);
#3494=LINE('',#19931,#4665);
#3495=LINE('',#19933,#4666);
#3496=LINE('',#19934,#4667);
#3497=LINE('',#19937,#4668);
#3498=LINE('',#19939,#4669);
#3499=LINE('',#19940,#4670);
#3500=LINE('',#19943,#4671);
#3501=LINE('',#19945,#4672);
#3502=LINE('',#19946,#4673);
#3503=LINE('',#19949,#4674);
#3504=LINE('',#19951,#4675);
#3505=LINE('',#19952,#4676);
#3506=LINE('',#19955,#4677);
#3507=LINE('',#19957,#4678);
#3508=LINE('',#19958,#4679);
#3509=LINE('',#19961,#4680);
#3510=LINE('',#19963,#4681);
#3511=LINE('',#19964,#4682);
#3512=LINE('',#19967,#4683);
#3513=LINE('',#19969,#4684);
#3514=LINE('',#19970,#4685);
#3515=LINE('',#19973,#4686);
#3516=LINE('',#19975,#4687);
#3517=LINE('',#19976,#4688);
#3518=LINE('',#19979,#4689);
#3519=LINE('',#19981,#4690);
#3520=LINE('',#19982,#4691);
#3521=LINE('',#19985,#4692);
#3522=LINE('',#19987,#4693);
#3523=LINE('',#19988,#4694);
#3524=LINE('',#19991,#4695);
#3525=LINE('',#19993,#4696);
#3526=LINE('',#19994,#4697);
#3527=LINE('',#19997,#4698);
#3528=LINE('',#19999,#4699);
#3529=LINE('',#20000,#4700);
#3530=LINE('',#20003,#4701);
#3531=LINE('',#20005,#4702);
#3532=LINE('',#20006,#4703);
#3533=LINE('',#20009,#4704);
#3534=LINE('',#20011,#4705);
#3535=LINE('',#20012,#4706);
#3536=LINE('',#20015,#4707);
#3537=LINE('',#20017,#4708);
#3538=LINE('',#20018,#4709);
#3539=LINE('',#20021,#4710);
#3540=LINE('',#20023,#4711);
#3541=LINE('',#20024,#4712);
#3542=LINE('',#20027,#4713);
#3543=LINE('',#20029,#4714);
#3544=LINE('',#20030,#4715);
#3545=LINE('',#20033,#4716);
#3546=LINE('',#20035,#4717);
#3547=LINE('',#20036,#4718);
#3548=LINE('',#20039,#4719);
#3549=LINE('',#20041,#4720);
#3550=LINE('',#20042,#4721);
#3551=LINE('',#20045,#4722);
#3552=LINE('',#20047,#4723);
#3553=LINE('',#20048,#4724);
#3554=LINE('',#20051,#4725);
#3555=LINE('',#20053,#4726);
#3556=LINE('',#20054,#4727);
#3557=LINE('',#20057,#4728);
#3558=LINE('',#20059,#4729);
#3559=LINE('',#20060,#4730);
#3560=LINE('',#20063,#4731);
#3561=LINE('',#20065,#4732);
#3562=LINE('',#20066,#4733);
#3563=LINE('',#20069,#4734);
#3564=LINE('',#20071,#4735);
#3565=LINE('',#20072,#4736);
#3566=LINE('',#20075,#4737);
#3567=LINE('',#20077,#4738);
#3568=LINE('',#20078,#4739);
#3569=LINE('',#20081,#4740);
#3570=LINE('',#20083,#4741);
#3571=LINE('',#20084,#4742);
#3572=LINE('',#20087,#4743);
#3573=LINE('',#20089,#4744);
#3574=LINE('',#20090,#4745);
#3575=LINE('',#20093,#4746);
#3576=LINE('',#20095,#4747);
#3577=LINE('',#20096,#4748);
#3578=LINE('',#20099,#4749);
#3579=LINE('',#20101,#4750);
#3580=LINE('',#20102,#4751);
#3581=LINE('',#20105,#4752);
#3582=LINE('',#20107,#4753);
#3583=LINE('',#20108,#4754);
#3584=LINE('',#20111,#4755);
#3585=LINE('',#20113,#4756);
#3586=LINE('',#20114,#4757);
#3587=LINE('',#20117,#4758);
#3588=LINE('',#20119,#4759);
#3589=LINE('',#20120,#4760);
#3590=LINE('',#20123,#4761);
#3591=LINE('',#20125,#4762);
#3592=LINE('',#20126,#4763);
#3593=LINE('',#20129,#4764);
#3594=LINE('',#20131,#4765);
#3595=LINE('',#20132,#4766);
#3596=LINE('',#20135,#4767);
#3597=LINE('',#20137,#4768);
#3598=LINE('',#20138,#4769);
#3599=LINE('',#20141,#4770);
#3600=LINE('',#20143,#4771);
#3601=LINE('',#20144,#4772);
#3602=LINE('',#20147,#4773);
#3603=LINE('',#20149,#4774);
#3604=LINE('',#20150,#4775);
#3605=LINE('',#20153,#4776);
#3606=LINE('',#20155,#4777);
#3607=LINE('',#20156,#4778);
#3608=LINE('',#20159,#4779);
#3609=LINE('',#20161,#4780);
#3610=LINE('',#20162,#4781);
#3611=LINE('',#20165,#4782);
#3612=LINE('',#20167,#4783);
#3613=LINE('',#20168,#4784);
#3614=LINE('',#20171,#4785);
#3615=LINE('',#20173,#4786);
#3616=LINE('',#20174,#4787);
#3617=LINE('',#20177,#4788);
#3618=LINE('',#20179,#4789);
#3619=LINE('',#20180,#4790);
#3620=LINE('',#20183,#4791);
#3621=LINE('',#20185,#4792);
#3622=LINE('',#20186,#4793);
#3623=LINE('',#20189,#4794);
#3624=LINE('',#20191,#4795);
#3625=LINE('',#20192,#4796);
#3626=LINE('',#20195,#4797);
#3627=LINE('',#20197,#4798);
#3628=LINE('',#20198,#4799);
#3629=LINE('',#20201,#4800);
#3630=LINE('',#20203,#4801);
#3631=LINE('',#20204,#4802);
#3632=LINE('',#20207,#4803);
#3633=LINE('',#20209,#4804);
#3634=LINE('',#20210,#4805);
#3635=LINE('',#20213,#4806);
#3636=LINE('',#20215,#4807);
#3637=LINE('',#20216,#4808);
#3638=LINE('',#20219,#4809);
#3639=LINE('',#20221,#4810);
#3640=LINE('',#20222,#4811);
#3641=LINE('',#20225,#4812);
#3642=LINE('',#20227,#4813);
#3643=LINE('',#20228,#4814);
#3644=LINE('',#20231,#4815);
#3645=LINE('',#20233,#4816);
#3646=LINE('',#20234,#4817);
#3647=LINE('',#20237,#4818);
#3648=LINE('',#20239,#4819);
#3649=LINE('',#20240,#4820);
#3650=LINE('',#20243,#4821);
#3651=LINE('',#20245,#4822);
#3652=LINE('',#20246,#4823);
#3653=LINE('',#20249,#4824);
#3654=LINE('',#20251,#4825);
#3655=LINE('',#20252,#4826);
#3656=LINE('',#20255,#4827);
#3657=LINE('',#20257,#4828);
#3658=LINE('',#20258,#4829);
#3659=LINE('',#20261,#4830);
#3660=LINE('',#20263,#4831);
#3661=LINE('',#20264,#4832);
#3662=LINE('',#20267,#4833);
#3663=LINE('',#20269,#4834);
#3664=LINE('',#20270,#4835);
#3665=LINE('',#20273,#4836);
#3666=LINE('',#20275,#4837);
#3667=LINE('',#20276,#4838);
#3668=LINE('',#20279,#4839);
#3669=LINE('',#20281,#4840);
#3670=LINE('',#20282,#4841);
#3671=LINE('',#20285,#4842);
#3672=LINE('',#20287,#4843);
#3673=LINE('',#20288,#4844);
#3674=LINE('',#20291,#4845);
#3675=LINE('',#20293,#4846);
#3676=LINE('',#20294,#4847);
#3677=LINE('',#20297,#4848);
#3678=LINE('',#20299,#4849);
#3679=LINE('',#20300,#4850);
#3680=LINE('',#20303,#4851);
#3681=LINE('',#20305,#4852);
#3682=LINE('',#20306,#4853);
#3683=LINE('',#20309,#4854);
#3684=LINE('',#20311,#4855);
#3685=LINE('',#20312,#4856);
#3686=LINE('',#20315,#4857);
#3687=LINE('',#20317,#4858);
#3688=LINE('',#20318,#4859);
#3689=LINE('',#20320,#4860);
#3690=LINE('',#20321,#4861);
#3691=LINE('',#20327,#4862);
#3692=LINE('',#20329,#4863);
#3693=LINE('',#20338,#4864);
#3694=LINE('',#20345,#4865);
#3695=LINE('',#20390,#4866);
#3696=LINE('',#20431,#4867);
#3697=LINE('',#20433,#4868);
#3698=LINE('',#20435,#4869);
#3699=LINE('',#20436,#4870);
#3700=LINE('',#20440,#4871);
#3701=LINE('',#20442,#4872);
#3702=LINE('',#20444,#4873);
#3703=LINE('',#20445,#4874);
#3704=LINE('',#20448,#4875);
#3705=LINE('',#20450,#4876);
#3706=LINE('',#20451,#4877);
#3707=LINE('',#20454,#4878);
#3708=LINE('',#20456,#4879);
#3709=LINE('',#20457,#4880);
#3710=LINE('',#20470,#4881);
#3711=LINE('',#20472,#4882);
#3712=LINE('',#20474,#4883);
#3713=LINE('',#20475,#4884);
#3714=LINE('',#20478,#4885);
#3715=LINE('',#20480,#4886);
#3716=LINE('',#20481,#4887);
#3717=LINE('',#20484,#4888);
#3718=LINE('',#20486,#4889);
#3719=LINE('',#20487,#4890);
#3720=LINE('',#20490,#4891);
#3721=LINE('',#20492,#4892);
#3722=LINE('',#20493,#4893);
#3723=LINE('',#20496,#4894);
#3724=LINE('',#20498,#4895);
#3725=LINE('',#20499,#4896);
#3726=LINE('',#20501,#4897);
#3727=LINE('',#20502,#4898);
#3728=LINE('',#20510,#4899);
#3729=LINE('',#20514,#4900);
#3730=LINE('',#20518,#4901);
#3731=LINE('',#20530,#4902);
#3732=LINE('',#20537,#4903);
#3733=LINE('',#20543,#4904);
#3734=LINE('',#20545,#4905);
#3735=LINE('',#20547,#4906);
#3736=LINE('',#20548,#4907);
#3737=LINE('',#20553,#4908);
#3738=LINE('',#20554,#4909);
#3739=LINE('',#20557,#4910);
#3740=LINE('',#20558,#4911);
#3741=LINE('',#20561,#4912);
#3742=LINE('',#20562,#4913);
#3743=LINE('',#20568,#4914);
#3744=LINE('',#20570,#4915);
#3745=LINE('',#20572,#4916);
#3746=LINE('',#20573,#4917);
#3747=LINE('',#20578,#4918);
#3748=LINE('',#20579,#4919);
#3749=LINE('',#20582,#4920);
#3750=LINE('',#20583,#4921);
#3751=LINE('',#20586,#4922);
#3752=LINE('',#20587,#4923);
#3753=LINE('',#20594,#4924);
#3754=LINE('',#20603,#4925);
#3755=LINE('',#20609,#4926);
#3756=LINE('',#20618,#4927);
#3757=LINE('',#20624,#4928);
#3758=LINE('',#20633,#4929);
#3759=LINE('',#20639,#4930);
#3760=LINE('',#20648,#4931);
#3761=LINE('',#20654,#4932);
#3762=LINE('',#20662,#4933);
#3763=LINE('',#20664,#4934);
#3764=LINE('',#20666,#4935);
#3765=LINE('',#20667,#4936);
#3766=LINE('',#20670,#4937);
#3767=LINE('',#20672,#4938);
#3768=LINE('',#20673,#4939);
#3769=LINE('',#20676,#4940);
#3770=LINE('',#20678,#4941);
#3771=LINE('',#20679,#4942);
#3772=LINE('',#20681,#4943);
#3773=LINE('',#20682,#4944);
#3774=LINE('',#20689,#4945);
#3775=LINE('',#20691,#4946);
#3776=LINE('',#20693,#4947);
#3777=LINE('',#20694,#4948);
#3778=LINE('',#20697,#4949);
#3779=LINE('',#20699,#4950);
#3780=LINE('',#20700,#4951);
#3781=LINE('',#20703,#4952);
#3782=LINE('',#20705,#4953);
#3783=LINE('',#20706,#4954);
#3784=LINE('',#20708,#4955);
#3785=LINE('',#20709,#4956);
#3786=LINE('',#20717,#4957);
#3787=LINE('',#20722,#4958);
#3788=LINE('',#20724,#4959);
#3789=LINE('',#20726,#4960);
#3790=LINE('',#20727,#4961);
#3791=LINE('',#20730,#4962);
#3792=LINE('',#20732,#4963);
#3793=LINE('',#20733,#4964);
#3794=LINE('',#20736,#4965);
#3795=LINE('',#20738,#4966);
#3796=LINE('',#20739,#4967);
#3797=LINE('',#20749,#4968);
#3798=LINE('',#20753,#4969);
#3799=LINE('',#20757,#4970);
#3800=LINE('',#20759,#4971);
#3801=LINE('',#20760,#4972);
#3802=LINE('',#20763,#4973);
#3803=LINE('',#20767,#4974);
#3804=LINE('',#20768,#4975);
#3805=LINE('',#20773,#4976);
#3806=LINE('',#20781,#4977);
#3807=LINE('',#20787,#4978);
#3808=LINE('',#20796,#4979);
#3809=LINE('',#20802,#4980);
#3810=LINE('',#20811,#4981);
#3811=LINE('',#20817,#4982);
#3812=LINE('',#20825,#4983);
#3813=LINE('',#20827,#4984);
#3814=LINE('',#20829,#4985);
#3815=LINE('',#20830,#4986);
#3816=LINE('',#20833,#4987);
#3817=LINE('',#20835,#4988);
#3818=LINE('',#20836,#4989);
#3819=LINE('',#20839,#4990);
#3820=LINE('',#20841,#4991);
#3821=LINE('',#20842,#4992);
#3822=LINE('',#20919,#4993);
#3823=LINE('',#21065,#4994);
#3824=LINE('',#21211,#4995);
#3825=LINE('',#21357,#4996);
#3826=LINE('',#21503,#4997);
#3827=LINE('',#21649,#4998);
#3828=LINE('',#21795,#4999);
#3829=LINE('',#21941,#5000);
#3830=LINE('',#22087,#5001);
#3831=LINE('',#22233,#5002);
#3832=LINE('',#22379,#5003);
#3833=LINE('',#22525,#5004);
#3834=LINE('',#22671,#5005);
#3835=LINE('',#22817,#5006);
#3836=LINE('',#22963,#5007);
#3837=LINE('',#23109,#5008);
#3838=LINE('',#23255,#5009);
#3839=LINE('',#23401,#5010);
#3840=LINE('',#23547,#5011);
#3841=LINE('',#23693,#5012);
#3842=LINE('',#23771,#5013);
#3843=LINE('',#23915,#5014);
#3844=LINE('',#23987,#5015);
#3845=LINE('',#23990,#5016);
#3846=LINE('',#23991,#5017);
#3847=LINE('',#24203,#5018);
#3848=LINE('',#24207,#5019);
#3849=LINE('',#24419,#5020);
#3850=LINE('',#24422,#5021);
#3851=LINE('',#24423,#5022);
#3852=LINE('',#24635,#5023);
#3853=LINE('',#24639,#5024);
#3854=LINE('',#24851,#5025);
#3855=LINE('',#24854,#5026);
#3856=LINE('',#24855,#5027);
#3857=LINE('',#25067,#5028);
#3858=LINE('',#25071,#5029);
#3859=LINE('',#25283,#5030);
#3860=LINE('',#25286,#5031);
#3861=LINE('',#25287,#5032);
#3862=LINE('',#25499,#5033);
#3863=LINE('',#25503,#5034);
#3864=LINE('',#25715,#5035);
#3865=LINE('',#25718,#5036);
#3866=LINE('',#25719,#5037);
#3867=LINE('',#25931,#5038);
#3868=LINE('',#25935,#5039);
#3869=LINE('',#26147,#5040);
#3870=LINE('',#26150,#5041);
#3871=LINE('',#26151,#5042);
#3872=LINE('',#26363,#5043);
#3873=LINE('',#26367,#5044);
#3874=LINE('',#26579,#5045);
#3875=LINE('',#26582,#5046);
#3876=LINE('',#26583,#5047);
#3877=LINE('',#26795,#5048);
#3878=LINE('',#26799,#5049);
#3879=LINE('',#27011,#5050);
#3880=LINE('',#27014,#5051);
#3881=LINE('',#27015,#5052);
#3882=LINE('',#27227,#5053);
#3883=LINE('',#27231,#5054);
#3884=LINE('',#27443,#5055);
#3885=LINE('',#27446,#5056);
#3886=LINE('',#27447,#5057);
#3887=LINE('',#27659,#5058);
#3888=LINE('',#27663,#5059);
#3889=LINE('',#27875,#5060);
#3890=LINE('',#27878,#5061);
#3891=LINE('',#27879,#5062);
#3892=LINE('',#28091,#5063);
#3893=LINE('',#28095,#5064);
#3894=LINE('',#28307,#5065);
#3895=LINE('',#28310,#5066);
#3896=LINE('',#28311,#5067);
#3897=LINE('',#28523,#5068);
#3898=LINE('',#28527,#5069);
#3899=LINE('',#28739,#5070);
#3900=LINE('',#28742,#5071);
#3901=LINE('',#28743,#5072);
#3902=LINE('',#28955,#5073);
#3903=LINE('',#28959,#5074);
#3904=LINE('',#29171,#5075);
#3905=LINE('',#29174,#5076);
#3906=LINE('',#29175,#5077);
#3907=LINE('',#29387,#5078);
#3908=LINE('',#29391,#5079);
#3909=LINE('',#29603,#5080);
#3910=LINE('',#29606,#5081);
#3911=LINE('',#29607,#5082);
#3912=LINE('',#29819,#5083);
#3913=LINE('',#29823,#5084);
#3914=LINE('',#30035,#5085);
#3915=LINE('',#30038,#5086);
#3916=LINE('',#30039,#5087);
#3917=LINE('',#30251,#5088);
#3918=LINE('',#30255,#5089);
#3919=LINE('',#30467,#5090);
#3920=LINE('',#30470,#5091);
#3921=LINE('',#30471,#5092);
#3922=LINE('',#30683,#5093);
#3923=LINE('',#30687,#5094);
#3924=LINE('',#30899,#5095);
#3925=LINE('',#30902,#5096);
#3926=LINE('',#30903,#5097);
#3927=LINE('',#31115,#5098);
#3928=LINE('',#31119,#5099);
#3929=LINE('',#31331,#5100);
#3930=LINE('',#31334,#5101);
#3931=LINE('',#31335,#5102);
#3932=LINE('',#31547,#5103);
#3933=LINE('',#31551,#5104);
#3934=LINE('',#31763,#5105);
#3935=LINE('',#31766,#5106);
#3936=LINE('',#31767,#5107);
#3937=LINE('',#31979,#5108);
#3938=LINE('',#31983,#5109);
#3939=LINE('',#32195,#5110);
#3940=LINE('',#32198,#5111);
#3941=LINE('',#32199,#5112);
#3942=LINE('',#32411,#5113);
#3943=LINE('',#32420,#5114);
#3944=LINE('',#32426,#5115);
#3945=LINE('',#32437,#5116);
#3946=LINE('',#32441,#5117);
#3947=LINE('',#32445,#5118);
#3948=LINE('',#32452,#5119);
#3949=LINE('',#32456,#5120);
#3950=LINE('',#32460,#5121);
#3951=LINE('',#32465,#5122);
#3952=LINE('',#32467,#5123);
#3953=LINE('',#32469,#5124);
#3954=LINE('',#32470,#5125);
#3955=LINE('',#32473,#5126);
#3956=LINE('',#32475,#5127);
#3957=LINE('',#32476,#5128);
#3958=LINE('',#32479,#5129);
#3959=LINE('',#32481,#5130);
#3960=LINE('',#32482,#5131);
#3961=LINE('',#32485,#5132);
#3962=LINE('',#32487,#5133);
#3963=LINE('',#32488,#5134);
#3964=LINE('',#32491,#5135);
#3965=LINE('',#32493,#5136);
#3966=LINE('',#32494,#5137);
#3967=LINE('',#32496,#5138);
#3968=LINE('',#32497,#5139);
#3969=LINE('',#32507,#5140);
#3970=LINE('',#32511,#5141);
#3971=LINE('',#32515,#5142);
#3972=LINE('',#32522,#5143);
#3973=LINE('',#32526,#5144);
#3974=LINE('',#32530,#5145);
#3975=LINE('',#32535,#5146);
#3976=LINE('',#32537,#5147);
#3977=LINE('',#32539,#5148);
#3978=LINE('',#32540,#5149);
#3979=LINE('',#32543,#5150);
#3980=LINE('',#32545,#5151);
#3981=LINE('',#32546,#5152);
#3982=LINE('',#32549,#5153);
#3983=LINE('',#32551,#5154);
#3984=LINE('',#32552,#5155);
#3985=LINE('',#32555,#5156);
#3986=LINE('',#32557,#5157);
#3987=LINE('',#32558,#5158);
#3988=LINE('',#32561,#5159);
#3989=LINE('',#32563,#5160);
#3990=LINE('',#32564,#5161);
#3991=LINE('',#32566,#5162);
#3992=LINE('',#32567,#5163);
#3993=LINE('',#32639,#5164);
#3994=LINE('',#32645,#5165);
#3995=VECTOR('',#14165,0.165);
#3996=VECTOR('',#14172,0.165);
#3997=VECTOR('',#14179,0.165);
#3998=VECTOR('',#14186,0.165);
#3999=VECTOR('',#14193,0.165);
#4000=VECTOR('',#14200,0.165);
#4001=VECTOR('',#14207,0.21);
#4002=VECTOR('',#14214,0.21);
#4003=VECTOR('',#14221,0.21);
#4004=VECTOR('',#14228,0.21);
#4005=VECTOR('',#14233,1.);
#4006=VECTOR('',#14234,1.);
#4007=VECTOR('',#14235,1.);
#4008=VECTOR('',#14236,1.);
#4009=VECTOR('',#14239,1.);
#4010=VECTOR('',#14240,1.);
#4011=VECTOR('',#14241,1.);
#4012=VECTOR('',#14244,1.);
#4013=VECTOR('',#14245,1.);
#4014=VECTOR('',#14246,1.);
#4015=VECTOR('',#14249,1.);
#4016=VECTOR('',#14250,1.);
#4017=VECTOR('',#14259,1.);
#4018=VECTOR('',#14260,1.);
#4019=VECTOR('',#14261,1.);
#4020=VECTOR('',#14262,1.);
#4021=VECTOR('',#14265,1.);
#4022=VECTOR('',#14266,1.);
#4023=VECTOR('',#14267,1.);
#4024=VECTOR('',#14270,1.);
#4025=VECTOR('',#14271,1.);
#4026=VECTOR('',#14272,1.);
#4027=VECTOR('',#14275,1.);
#4028=VECTOR('',#14276,1.);
#4029=VECTOR('',#14285,1.);
#4030=VECTOR('',#14286,1.);
#4031=VECTOR('',#14287,1.);
#4032=VECTOR('',#14288,1.);
#4033=VECTOR('',#14291,1.);
#4034=VECTOR('',#14292,1.);
#4035=VECTOR('',#14293,1.);
#4036=VECTOR('',#14296,1.);
#4037=VECTOR('',#14297,1.);
#4038=VECTOR('',#14298,1.);
#4039=VECTOR('',#14301,1.);
#4040=VECTOR('',#14302,1.);
#4041=VECTOR('',#14313,0.165);
#4042=VECTOR('',#14322,0.165);
#4043=VECTOR('',#14329,1.);
#4044=VECTOR('',#14330,1.);
#4045=VECTOR('',#14331,1.);
#4046=VECTOR('',#14332,1.);
#4047=VECTOR('',#14335,1.);
#4048=VECTOR('',#14336,1.);
#4049=VECTOR('',#14337,1.);
#4050=VECTOR('',#14338,1.);
#4051=VECTOR('',#14343,1.);
#4052=VECTOR('',#14344,1.);
#4053=VECTOR('',#14345,1.);
#4054=VECTOR('',#14356,1.);
#4055=VECTOR('',#14363,1.);
#4056=VECTOR('',#14366,1.);
#4057=VECTOR('',#14367,1.);
#4058=VECTOR('',#14368,1.);
#4059=VECTOR('',#14371,1.);
#4060=VECTOR('',#14374,1.);
#4061=VECTOR('',#14379,0.165);
#4062=VECTOR('',#14388,0.165);
#4063=VECTOR('',#14395,1.);
#4064=VECTOR('',#14396,1.);
#4065=VECTOR('',#14397,1.);
#4066=VECTOR('',#14398,1.);
#4067=VECTOR('',#14401,1.);
#4068=VECTOR('',#14402,1.);
#4069=VECTOR('',#14403,1.);
#4070=VECTOR('',#14404,1.);
#4071=VECTOR('',#14409,1.);
#4072=VECTOR('',#14410,1.);
#4073=VECTOR('',#14411,1.);
#4074=VECTOR('',#14422,1.);
#4075=VECTOR('',#14429,1.);
#4076=VECTOR('',#14432,1.);
#4077=VECTOR('',#14433,1.);
#4078=VECTOR('',#14434,1.);
#4079=VECTOR('',#14437,1.);
#4080=VECTOR('',#14440,1.);
#4081=VECTOR('',#14445,0.275);
#4082=VECTOR('',#14452,0.275);
#4083=VECTOR('',#14459,0.275);
#4084=VECTOR('',#14466,0.275);
#4085=VECTOR('',#14471,1.);
#4086=VECTOR('',#14472,1.);
#4087=VECTOR('',#14473,1.);
#4088=VECTOR('',#14474,1.);
#4089=VECTOR('',#14475,1.);
#4090=VECTOR('',#14476,1.);
#4091=VECTOR('',#14477,1.);
#4092=VECTOR('',#14478,1.);
#4093=VECTOR('',#14481,1.);
#4094=VECTOR('',#14482,1.);
#4095=VECTOR('',#14483,1.);
#4096=VECTOR('',#14486,1.);
#4097=VECTOR('',#14487,1.);
#4098=VECTOR('',#14490,1.);
#4099=VECTOR('',#14491,1.);
#4100=VECTOR('',#14494,1.);
#4101=VECTOR('',#14497,1.);
#4102=VECTOR('',#14498,1.);
#4103=VECTOR('',#14499,1.);
#4104=VECTOR('',#14502,1.);
#4105=VECTOR('',#14503,1.);
#4106=VECTOR('',#14506,1.);
#4107=VECTOR('',#14507,1.);
#4108=VECTOR('',#14510,1.);
#4109=VECTOR('',#14519,1.);
#4110=VECTOR('',#14520,1.);
#4111=VECTOR('',#14521,1.);
#4112=VECTOR('',#14522,1.);
#4113=VECTOR('',#14525,1.);
#4114=VECTOR('',#14526,1.);
#4115=VECTOR('',#14527,1.);
#4116=VECTOR('',#14528,1.);
#4117=VECTOR('',#14531,1.);
#4118=VECTOR('',#14532,1.);
#4119=VECTOR('',#14533,1.);
#4120=VECTOR('',#14534,1.);
#4121=VECTOR('',#14535,1.);
#4122=VECTOR('',#14538,1.);
#4123=VECTOR('',#14539,1.);
#4124=VECTOR('',#14540,1.);
#4125=VECTOR('',#14541,1.);
#4126=VECTOR('',#14542,1.);
#4127=VECTOR('',#14573,0.225);
#4128=VECTOR('',#14580,0.225);
#4129=VECTOR('',#14585,1.);
#4130=VECTOR('',#14586,1.);
#4131=VECTOR('',#14587,1.);
#4132=VECTOR('',#14588,1.);
#4133=VECTOR('',#14591,1.);
#4134=VECTOR('',#14592,1.);
#4135=VECTOR('',#14593,1.);
#4136=VECTOR('',#14594,1.);
#4137=VECTOR('',#14597,1.);
#4138=VECTOR('',#14598,1.);
#4139=VECTOR('',#14599,1.);
#4140=VECTOR('',#14602,1.);
#4141=VECTOR('',#14603,1.);
#4142=VECTOR('',#14604,1.);
#4143=VECTOR('',#14607,1.);
#4144=VECTOR('',#14608,1.);
#4145=VECTOR('',#14609,1.);
#4146=VECTOR('',#14612,1.);
#4147=VECTOR('',#14613,1.);
#4148=VECTOR('',#14614,1.);
#4149=VECTOR('',#14619,1.);
#4150=VECTOR('',#14620,1.);
#4151=VECTOR('',#14621,1.);
#4152=VECTOR('',#14628,1.);
#4153=VECTOR('',#14629,1.);
#4154=VECTOR('',#14632,1.);
#4155=VECTOR('',#14633,1.);
#4156=VECTOR('',#14636,1.);
#4157=VECTOR('',#14643,1.);
#4158=VECTOR('',#14644,1.);
#4159=VECTOR('',#14645,1.);
#4160=VECTOR('',#14646,1.);
#4161=VECTOR('',#14649,1.);
#4162=VECTOR('',#14650,1.);
#4163=VECTOR('',#14651,1.);
#4164=VECTOR('',#14652,1.);
#4165=VECTOR('',#14655,1.);
#4166=VECTOR('',#14656,1.);
#4167=VECTOR('',#14657,1.);
#4168=VECTOR('',#14658,1.);
#4169=VECTOR('',#14659,1.);
#4170=VECTOR('',#14662,1.);
#4171=VECTOR('',#14663,1.);
#4172=VECTOR('',#14664,1.);
#4173=VECTOR('',#14665,1.);
#4174=VECTOR('',#14666,1.);
#4175=VECTOR('',#14697,0.225);
#4176=VECTOR('',#14704,0.225);
#4177=VECTOR('',#14709,1.);
#4178=VECTOR('',#14710,1.);
#4179=VECTOR('',#14711,1.);
#4180=VECTOR('',#14712,1.);
#4181=VECTOR('',#14715,1.);
#4182=VECTOR('',#14716,1.);
#4183=VECTOR('',#14717,1.);
#4184=VECTOR('',#14718,1.);
#4185=VECTOR('',#14721,1.);
#4186=VECTOR('',#14722,1.);
#4187=VECTOR('',#14723,1.);
#4188=VECTOR('',#14726,1.);
#4189=VECTOR('',#14727,1.);
#4190=VECTOR('',#14728,1.);
#4191=VECTOR('',#14731,1.);
#4192=VECTOR('',#14732,1.);
#4193=VECTOR('',#14733,1.);
#4194=VECTOR('',#14736,1.);
#4195=VECTOR('',#14737,1.);
#4196=VECTOR('',#14738,1.);
#4197=VECTOR('',#14743,1.);
#4198=VECTOR('',#14744,1.);
#4199=VECTOR('',#14745,1.);
#4200=VECTOR('',#14752,1.);
#4201=VECTOR('',#14753,1.);
#4202=VECTOR('',#14756,1.);
#4203=VECTOR('',#14757,1.);
#4204=VECTOR('',#14760,1.);
#4205=VECTOR('',#14769,0.4);
#4206=VECTOR('',#14780,0.4);
#4207=VECTOR('',#14791,0.225);
#4208=VECTOR('',#14796,0.225);
#4209=VECTOR('',#14801,2.5);
#4210=VECTOR('',#14814,1.);
#4211=VECTOR('',#14817,1.);
#4212=VECTOR('',#14820,1.);
#4213=VECTOR('',#14821,1.);
#4214=VECTOR('',#14822,1.);
#4215=VECTOR('',#14823,1.);
#4216=VECTOR('',#14830,1.);
#4217=VECTOR('',#14831,1.);
#4218=VECTOR('',#14836,0.165);
#4219=VECTOR('',#14843,0.165);
#4220=VECTOR('',#14850,0.165);
#4221=VECTOR('',#14857,0.165);
#4222=VECTOR('',#14862,0.225);
#4223=VECTOR('',#14867,0.225);
#4224=VECTOR('',#14874,1.6);
#4225=VECTOR('',#14879,1.);
#4226=VECTOR('',#14880,1.);
#4227=VECTOR('',#14881,1.);
#4228=VECTOR('',#14884,1.);
#4229=VECTOR('',#14885,1.);
#4230=VECTOR('',#14886,1.);
#4231=VECTOR('',#14887,1.);
#4232=VECTOR('',#14890,1.);
#4233=VECTOR('',#14891,1.);
#4234=VECTOR('',#14894,1.);
#4235=VECTOR('',#14895,1.);
#4236=VECTOR('',#14896,1.);
#4237=VECTOR('',#14899,1.);
#4238=VECTOR('',#14900,1.);
#4239=VECTOR('',#14903,1.);
#4240=VECTOR('',#14904,1.);
#4241=VECTOR('',#14907,1.);
#4242=VECTOR('',#14916,1.41);
#4243=VECTOR('',#14923,0.225);
#4244=VECTOR('',#14930,0.225);
#4245=VECTOR('',#14937,0.225);
#4246=VECTOR('',#14944,0.225);
#4247=VECTOR('',#14951,1.59);
#4248=VECTOR('',#14960,2.4);
#4249=VECTOR('',#14973,1.41);
#4250=VECTOR('',#14980,0.225);
#4251=VECTOR('',#14987,0.225);
#4252=VECTOR('',#14994,0.225);
#4253=VECTOR('',#15001,0.225);
#4254=VECTOR('',#15008,1.59);
#4255=VECTOR('',#15017,2.4);
#4256=VECTOR('',#15030,1.);
#4257=VECTOR('',#15033,1.);
#4258=VECTOR('',#15036,1.);
#4259=VECTOR('',#15037,1.);
#4260=VECTOR('',#15038,1.);
#4261=VECTOR('',#15039,1.);
#4262=VECTOR('',#15046,1.);
#4263=VECTOR('',#15047,1.);
#4264=VECTOR('',#15048,1.);
#4265=VECTOR('',#15049,1.);
#4266=VECTOR('',#15050,1.);
#4267=VECTOR('',#15051,1.);
#4268=VECTOR('',#15064,0.165);
#4269=VECTOR('',#15069,0.165);
#4270=VECTOR('',#15074,0.165);
#4271=VECTOR('',#15079,0.165);
#4272=VECTOR('',#15084,0.225);
#4273=VECTOR('',#15089,0.225);
#4274=VECTOR('',#15094,1.6);
#4275=VECTOR('',#15099,1.);
#4276=VECTOR('',#15100,1.);
#4277=VECTOR('',#15101,1.);
#4278=VECTOR('',#15104,1.);
#4279=VECTOR('',#15105,1.);
#4280=VECTOR('',#15106,1.);
#4281=VECTOR('',#15109,1.);
#4282=VECTOR('',#15112,1.);
#4283=VECTOR('',#15115,1.);
#4284=VECTOR('',#15116,1.);
#4285=VECTOR('',#15119,1.);
#4286=VECTOR('',#15120,1.);
#4287=VECTOR('',#15123,1.);
#4288=VECTOR('',#15132,1.41);
#4289=VECTOR('',#15139,0.225);
#4290=VECTOR('',#15146,0.225);
#4291=VECTOR('',#15153,0.225);
#4292=VECTOR('',#15160,0.225);
#4293=VECTOR('',#15167,1.59);
#4294=VECTOR('',#15176,2.4);
#4295=VECTOR('',#15189,1.41);
#4296=VECTOR('',#15196,0.225);
#4297=VECTOR('',#15203,0.225);
#4298=VECTOR('',#15210,0.225);
#4299=VECTOR('',#15217,0.225);
#4300=VECTOR('',#15224,1.59);
#4301=VECTOR('',#15233,2.4);
#4302=VECTOR('',#15250,0.4);
#4303=VECTOR('',#15255,0.425);
#4304=VECTOR('',#15260,0.41);
#4305=VECTOR('',#15269,0.26);
#4306=VECTOR('',#15274,0.25);
#4307=VECTOR('',#15279,0.225);
#4308=VECTOR('',#15284,1.);
#4309=VECTOR('',#15285,1.);
#4310=VECTOR('',#15286,1.);
#4311=VECTOR('',#15287,1.);
#4312=VECTOR('',#15290,1.);
#4313=VECTOR('',#15291,1.);
#4314=VECTOR('',#15292,1.);
#4315=VECTOR('',#15295,1.);
#4316=VECTOR('',#15296,1.);
#4317=VECTOR('',#15297,1.);
#4318=VECTOR('',#15300,1.);
#4319=VECTOR('',#15301,1.);
#4320=VECTOR('',#15302,1.);
#4321=VECTOR('',#15305,1.);
#4322=VECTOR('',#15306,1.);
#4323=VECTOR('',#15307,1.);
#4324=VECTOR('',#15310,1.);
#4325=VECTOR('',#15311,1.);
#4326=VECTOR('',#15334,1.070235);
#4327=VECTOR('',#15341,0.6);
#4328=VECTOR('',#15346,0.63);
#4329=VECTOR('',#15355,1.070235);
#4330=VECTOR('',#15362,0.63);
#4331=VECTOR('',#15381,1.129765);
#4332=VECTOR('',#15392,1.57);
#4333=VECTOR('',#15397,1.6);
#4334=VECTOR('',#15402,1.57);
#4335=VECTOR('',#15407,1.129765);
#4336=VECTOR('',#15454,1.123812);
#4337=VECTOR('',#15523,1.076188);
#4338=VECTOR('',#15552,1.119765);
#4339=VECTOR('',#15559,1.085235);
#4340=VECTOR('',#15570,1.119765);
#4341=VECTOR('',#15577,1.085235);
#4342=VECTOR('',#15592,1.);
#4343=VECTOR('',#15593,1.);
#4344=VECTOR('',#15594,1.);
#4345=VECTOR('',#15595,1.);
#4346=VECTOR('',#15598,1.);
#4347=VECTOR('',#15599,1.);
#4348=VECTOR('',#15600,1.);
#4349=VECTOR('',#15603,1.);
#4350=VECTOR('',#15604,1.);
#4351=VECTOR('',#15605,1.);
#4352=VECTOR('',#15608,1.);
#4353=VECTOR('',#15609,1.);
#4354=VECTOR('',#15610,1.);
#4355=VECTOR('',#15613,1.);
#4356=VECTOR('',#15614,1.);
#4357=VECTOR('',#15615,1.);
#4358=VECTOR('',#15618,1.);
#4359=VECTOR('',#15619,1.);
#4360=VECTOR('',#15636,0.325);
#4361=VECTOR('',#15641,0.35);
#4362=VECTOR('',#15646,0.335);
#4363=VECTOR('',#15655,0.21);
#4364=VECTOR('',#15658,0.2);
#4365=VECTOR('',#15667,0.425);
#4366=VECTOR('',#15674,1.);
#4367=VECTOR('',#15675,1.);
#4368=VECTOR('',#15676,1.);
#4369=VECTOR('',#15677,1.);
#4370=VECTOR('',#15680,1.);
#4371=VECTOR('',#15681,1.);
#4372=VECTOR('',#15682,1.);
#4373=VECTOR('',#15683,1.);
#4374=VECTOR('',#15688,1.);
#4375=VECTOR('',#15689,1.);
#4376=VECTOR('',#15690,1.);
#4377=VECTOR('',#15697,1.);
#4378=VECTOR('',#15698,1.);
#4379=VECTOR('',#15699,1.);
#4380=VECTOR('',#15704,1.);
#4381=VECTOR('',#15705,1.);
#4382=VECTOR('',#15706,1.);
#4383=VECTOR('',#15709,1.);
#4384=VECTOR('',#15710,1.);
#4385=VECTOR('',#15711,1.);
#4386=VECTOR('',#15714,1.);
#4387=VECTOR('',#15715,1.);
#4388=VECTOR('',#15716,1.);
#4389=VECTOR('',#15719,1.);
#4390=VECTOR('',#15720,1.);
#4391=VECTOR('',#15721,1.);
#4392=VECTOR('',#15724,1.);
#4393=VECTOR('',#15725,1.);
#4394=VECTOR('',#15726,1.);
#4395=VECTOR('',#15729,1.);
#4396=VECTOR('',#15730,1.);
#4397=VECTOR('',#15731,1.);
#4398=VECTOR('',#15734,1.);
#4399=VECTOR('',#15735,1.);
#4400=VECTOR('',#15736,1.);
#4401=VECTOR('',#15739,1.);
#4402=VECTOR('',#15740,1.);
#4403=VECTOR('',#15741,1.);
#4404=VECTOR('',#15744,1.);
#4405=VECTOR('',#15745,1.);
#4406=VECTOR('',#15746,1.);
#4407=VECTOR('',#15749,1.);
#4408=VECTOR('',#15750,1.);
#4409=VECTOR('',#15751,1.);
#4410=VECTOR('',#15754,1.);
#4411=VECTOR('',#15755,1.);
#4412=VECTOR('',#15756,1.);
#4413=VECTOR('',#15759,1.);
#4414=VECTOR('',#15760,1.);
#4415=VECTOR('',#15761,1.);
#4416=VECTOR('',#15764,1.);
#4417=VECTOR('',#15765,1.);
#4418=VECTOR('',#15766,1.);
#4419=VECTOR('',#15769,1.);
#4420=VECTOR('',#15770,1.);
#4421=VECTOR('',#15771,1.);
#4422=VECTOR('',#15774,1.);
#4423=VECTOR('',#15775,1.);
#4424=VECTOR('',#15776,1.);
#4425=VECTOR('',#15779,1.);
#4426=VECTOR('',#15780,1.);
#4427=VECTOR('',#15781,1.);
#4428=VECTOR('',#15784,1.);
#4429=VECTOR('',#15785,1.);
#4430=VECTOR('',#15786,1.);
#4431=VECTOR('',#15789,1.);
#4432=VECTOR('',#15790,1.);
#4433=VECTOR('',#15791,1.);
#4434=VECTOR('',#15794,1.);
#4435=VECTOR('',#15795,1.);
#4436=VECTOR('',#15796,1.);
#4437=VECTOR('',#15799,1.);
#4438=VECTOR('',#15800,1.);
#4439=VECTOR('',#15801,1.);
#4440=VECTOR('',#15804,1.);
#4441=VECTOR('',#15805,1.);
#4442=VECTOR('',#15806,1.);
#4443=VECTOR('',#15809,1.);
#4444=VECTOR('',#15810,1.);
#4445=VECTOR('',#15811,1.);
#4446=VECTOR('',#15814,1.);
#4447=VECTOR('',#15815,1.);
#4448=VECTOR('',#15816,1.);
#4449=VECTOR('',#15819,1.);
#4450=VECTOR('',#15820,1.);
#4451=VECTOR('',#15821,1.);
#4452=VECTOR('',#15824,1.);
#4453=VECTOR('',#15825,1.);
#4454=VECTOR('',#15826,1.);
#4455=VECTOR('',#15829,1.);
#4456=VECTOR('',#15830,1.);
#4457=VECTOR('',#15831,1.);
#4458=VECTOR('',#15834,1.);
#4459=VECTOR('',#15835,1.);
#4460=VECTOR('',#15836,1.);
#4461=VECTOR('',#15839,1.);
#4462=VECTOR('',#15840,1.);
#4463=VECTOR('',#15841,1.);
#4464=VECTOR('',#15844,1.);
#4465=VECTOR('',#15845,1.);
#4466=VECTOR('',#15846,1.);
#4467=VECTOR('',#15849,1.);
#4468=VECTOR('',#15850,1.);
#4469=VECTOR('',#15851,1.);
#4470=VECTOR('',#15854,1.);
#4471=VECTOR('',#15855,1.);
#4472=VECTOR('',#15856,1.);
#4473=VECTOR('',#15859,1.);
#4474=VECTOR('',#15860,1.);
#4475=VECTOR('',#15861,1.);
#4476=VECTOR('',#15864,1.);
#4477=VECTOR('',#15865,1.);
#4478=VECTOR('',#15866,1.);
#4479=VECTOR('',#15869,1.);
#4480=VECTOR('',#15870,1.);
#4481=VECTOR('',#15871,1.);
#4482=VECTOR('',#15874,1.);
#4483=VECTOR('',#15875,1.);
#4484=VECTOR('',#15876,1.);
#4485=VECTOR('',#15879,1.);
#4486=VECTOR('',#15880,1.);
#4487=VECTOR('',#15881,1.);
#4488=VECTOR('',#15884,1.);
#4489=VECTOR('',#15885,1.);
#4490=VECTOR('',#15886,1.);
#4491=VECTOR('',#15889,1.);
#4492=VECTOR('',#15890,1.);
#4493=VECTOR('',#15891,1.);
#4494=VECTOR('',#15894,1.);
#4495=VECTOR('',#15895,1.);
#4496=VECTOR('',#15896,1.);
#4497=VECTOR('',#15899,1.);
#4498=VECTOR('',#15900,1.);
#4499=VECTOR('',#15901,1.);
#4500=VECTOR('',#15904,1.);
#4501=VECTOR('',#15905,1.);
#4502=VECTOR('',#15906,1.);
#4503=VECTOR('',#15909,1.);
#4504=VECTOR('',#15910,1.);
#4505=VECTOR('',#15911,1.);
#4506=VECTOR('',#15914,1.);
#4507=VECTOR('',#15915,1.);
#4508=VECTOR('',#15916,1.);
#4509=VECTOR('',#15919,1.);
#4510=VECTOR('',#15920,1.);
#4511=VECTOR('',#15921,1.);
#4512=VECTOR('',#15924,1.);
#4513=VECTOR('',#15925,1.);
#4514=VECTOR('',#15926,1.);
#4515=VECTOR('',#15929,1.);
#4516=VECTOR('',#15930,1.);
#4517=VECTOR('',#15931,1.);
#4518=VECTOR('',#15934,1.);
#4519=VECTOR('',#15935,1.);
#4520=VECTOR('',#15936,1.);
#4521=VECTOR('',#15939,1.);
#4522=VECTOR('',#15940,1.);
#4523=VECTOR('',#15941,1.);
#4524=VECTOR('',#15944,1.);
#4525=VECTOR('',#15945,1.);
#4526=VECTOR('',#15946,1.);
#4527=VECTOR('',#15949,1.);
#4528=VECTOR('',#15950,1.);
#4529=VECTOR('',#15951,1.);
#4530=VECTOR('',#15954,1.);
#4531=VECTOR('',#15955,1.);
#4532=VECTOR('',#15956,1.);
#4533=VECTOR('',#15959,1.);
#4534=VECTOR('',#15960,1.);
#4535=VECTOR('',#15961,1.);
#4536=VECTOR('',#15964,1.);
#4537=VECTOR('',#15965,1.);
#4538=VECTOR('',#15966,1.);
#4539=VECTOR('',#15969,1.);
#4540=VECTOR('',#15970,1.);
#4541=VECTOR('',#15971,1.);
#4542=VECTOR('',#15974,1.);
#4543=VECTOR('',#15975,1.);
#4544=VECTOR('',#15976,1.);
#4545=VECTOR('',#15979,1.);
#4546=VECTOR('',#15980,1.);
#4547=VECTOR('',#15981,1.);
#4548=VECTOR('',#15984,1.);
#4549=VECTOR('',#15985,1.);
#4550=VECTOR('',#15986,1.);
#4551=VECTOR('',#15989,1.);
#4552=VECTOR('',#15990,1.);
#4553=VECTOR('',#15991,1.);
#4554=VECTOR('',#15994,1.);
#4555=VECTOR('',#15995,1.);
#4556=VECTOR('',#15996,1.);
#4557=VECTOR('',#15999,1.);
#4558=VECTOR('',#16000,1.);
#4559=VECTOR('',#16001,1.);
#4560=VECTOR('',#16004,1.);
#4561=VECTOR('',#16005,1.);
#4562=VECTOR('',#16006,1.);
#4563=VECTOR('',#16009,1.);
#4564=VECTOR('',#16010,1.);
#4565=VECTOR('',#16011,1.);
#4566=VECTOR('',#16014,1.);
#4567=VECTOR('',#16015,1.);
#4568=VECTOR('',#16016,1.);
#4569=VECTOR('',#16019,1.);
#4570=VECTOR('',#16020,1.);
#4571=VECTOR('',#16021,1.);
#4572=VECTOR('',#16024,1.);
#4573=VECTOR('',#16025,1.);
#4574=VECTOR('',#16026,1.);
#4575=VECTOR('',#16029,1.);
#4576=VECTOR('',#16030,1.);
#4577=VECTOR('',#16031,1.);
#4578=VECTOR('',#16034,1.);
#4579=VECTOR('',#16035,1.);
#4580=VECTOR('',#16036,1.);
#4581=VECTOR('',#16039,1.);
#4582=VECTOR('',#16040,1.);
#4583=VECTOR('',#16041,1.);
#4584=VECTOR('',#16044,1.);
#4585=VECTOR('',#16045,1.);
#4586=VECTOR('',#16046,1.);
#4587=VECTOR('',#16049,1.);
#4588=VECTOR('',#16050,1.);
#4589=VECTOR('',#16051,1.);
#4590=VECTOR('',#16054,1.);
#4591=VECTOR('',#16055,1.);
#4592=VECTOR('',#16056,1.);
#4593=VECTOR('',#16059,1.);
#4594=VECTOR('',#16060,1.);
#4595=VECTOR('',#16061,1.);
#4596=VECTOR('',#16064,1.);
#4597=VECTOR('',#16065,1.);
#4598=VECTOR('',#16066,1.);
#4599=VECTOR('',#16069,1.);
#4600=VECTOR('',#16070,1.);
#4601=VECTOR('',#16071,1.);
#4602=VECTOR('',#16074,1.);
#4603=VECTOR('',#16075,1.);
#4604=VECTOR('',#16076,1.);
#4605=VECTOR('',#16079,1.);
#4606=VECTOR('',#16080,1.);
#4607=VECTOR('',#16081,1.);
#4608=VECTOR('',#16084,1.);
#4609=VECTOR('',#16085,1.);
#4610=VECTOR('',#16086,1.);
#4611=VECTOR('',#16089,1.);
#4612=VECTOR('',#16090,1.);
#4613=VECTOR('',#16091,1.);
#4614=VECTOR('',#16094,1.);
#4615=VECTOR('',#16095,1.);
#4616=VECTOR('',#16096,1.);
#4617=VECTOR('',#16099,1.);
#4618=VECTOR('',#16100,1.);
#4619=VECTOR('',#16101,1.);
#4620=VECTOR('',#16104,1.);
#4621=VECTOR('',#16105,1.);
#4622=VECTOR('',#16106,1.);
#4623=VECTOR('',#16109,1.);
#4624=VECTOR('',#16110,1.);
#4625=VECTOR('',#16111,1.);
#4626=VECTOR('',#16114,1.);
#4627=VECTOR('',#16115,1.);
#4628=VECTOR('',#16116,1.);
#4629=VECTOR('',#16119,1.);
#4630=VECTOR('',#16120,1.);
#4631=VECTOR('',#16121,1.);
#4632=VECTOR('',#16124,1.);
#4633=VECTOR('',#16125,1.);
#4634=VECTOR('',#16126,1.);
#4635=VECTOR('',#16129,1.);
#4636=VECTOR('',#16130,1.);
#4637=VECTOR('',#16131,1.);
#4638=VECTOR('',#16134,1.);
#4639=VECTOR('',#16135,1.);
#4640=VECTOR('',#16136,1.);
#4641=VECTOR('',#16139,1.);
#4642=VECTOR('',#16140,1.);
#4643=VECTOR('',#16141,1.);
#4644=VECTOR('',#16144,1.);
#4645=VECTOR('',#16145,1.);
#4646=VECTOR('',#16146,1.);
#4647=VECTOR('',#16149,1.);
#4648=VECTOR('',#16150,1.);
#4649=VECTOR('',#16151,1.);
#4650=VECTOR('',#16154,1.);
#4651=VECTOR('',#16155,1.);
#4652=VECTOR('',#16156,1.);
#4653=VECTOR('',#16159,1.);
#4654=VECTOR('',#16160,1.);
#4655=VECTOR('',#16161,1.);
#4656=VECTOR('',#16164,1.);
#4657=VECTOR('',#16165,1.);
#4658=VECTOR('',#16166,1.);
#4659=VECTOR('',#16169,1.);
#4660=VECTOR('',#16170,1.);
#4661=VECTOR('',#16171,1.);
#4662=VECTOR('',#16174,1.);
#4663=VECTOR('',#16175,1.);
#4664=VECTOR('',#16176,1.);
#4665=VECTOR('',#16179,1.);
#4666=VECTOR('',#16180,1.);
#4667=VECTOR('',#16181,1.);
#4668=VECTOR('',#16184,1.);
#4669=VECTOR('',#16185,1.);
#4670=VECTOR('',#16186,1.);
#4671=VECTOR('',#16189,1.);
#4672=VECTOR('',#16190,1.);
#4673=VECTOR('',#16191,1.);
#4674=VECTOR('',#16194,1.);
#4675=VECTOR('',#16195,1.);
#4676=VECTOR('',#16196,1.);
#4677=VECTOR('',#16199,1.);
#4678=VECTOR('',#16200,1.);
#4679=VECTOR('',#16201,1.);
#4680=VECTOR('',#16204,1.);
#4681=VECTOR('',#16205,1.);
#4682=VECTOR('',#16206,1.);
#4683=VECTOR('',#16209,1.);
#4684=VECTOR('',#16210,1.);
#4685=VECTOR('',#16211,1.);
#4686=VECTOR('',#16214,1.);
#4687=VECTOR('',#16215,1.);
#4688=VECTOR('',#16216,1.);
#4689=VECTOR('',#16219,1.);
#4690=VECTOR('',#16220,1.);
#4691=VECTOR('',#16221,1.);
#4692=VECTOR('',#16224,1.);
#4693=VECTOR('',#16225,1.);
#4694=VECTOR('',#16226,1.);
#4695=VECTOR('',#16229,1.);
#4696=VECTOR('',#16230,1.);
#4697=VECTOR('',#16231,1.);
#4698=VECTOR('',#16234,1.);
#4699=VECTOR('',#16235,1.);
#4700=VECTOR('',#16236,1.);
#4701=VECTOR('',#16239,1.);
#4702=VECTOR('',#16240,1.);
#4703=VECTOR('',#16241,1.);
#4704=VECTOR('',#16244,1.);
#4705=VECTOR('',#16245,1.);
#4706=VECTOR('',#16246,1.);
#4707=VECTOR('',#16249,1.);
#4708=VECTOR('',#16250,1.);
#4709=VECTOR('',#16251,1.);
#4710=VECTOR('',#16254,1.);
#4711=VECTOR('',#16255,1.);
#4712=VECTOR('',#16256,1.);
#4713=VECTOR('',#16259,1.);
#4714=VECTOR('',#16260,1.);
#4715=VECTOR('',#16261,1.);
#4716=VECTOR('',#16264,1.);
#4717=VECTOR('',#16265,1.);
#4718=VECTOR('',#16266,1.);
#4719=VECTOR('',#16269,1.);
#4720=VECTOR('',#16270,1.);
#4721=VECTOR('',#16271,1.);
#4722=VECTOR('',#16274,1.);
#4723=VECTOR('',#16275,1.);
#4724=VECTOR('',#16276,1.);
#4725=VECTOR('',#16279,1.);
#4726=VECTOR('',#16280,1.);
#4727=VECTOR('',#16281,1.);
#4728=VECTOR('',#16284,1.);
#4729=VECTOR('',#16285,1.);
#4730=VECTOR('',#16286,1.);
#4731=VECTOR('',#16289,1.);
#4732=VECTOR('',#16290,1.);
#4733=VECTOR('',#16291,1.);
#4734=VECTOR('',#16294,1.);
#4735=VECTOR('',#16295,1.);
#4736=VECTOR('',#16296,1.);
#4737=VECTOR('',#16299,1.);
#4738=VECTOR('',#16300,1.);
#4739=VECTOR('',#16301,1.);
#4740=VECTOR('',#16304,1.);
#4741=VECTOR('',#16305,1.);
#4742=VECTOR('',#16306,1.);
#4743=VECTOR('',#16309,1.);
#4744=VECTOR('',#16310,1.);
#4745=VECTOR('',#16311,1.);
#4746=VECTOR('',#16314,1.);
#4747=VECTOR('',#16315,1.);
#4748=VECTOR('',#16316,1.);
#4749=VECTOR('',#16319,1.);
#4750=VECTOR('',#16320,1.);
#4751=VECTOR('',#16321,1.);
#4752=VECTOR('',#16324,1.);
#4753=VECTOR('',#16325,1.);
#4754=VECTOR('',#16326,1.);
#4755=VECTOR('',#16329,1.);
#4756=VECTOR('',#16330,1.);
#4757=VECTOR('',#16331,1.);
#4758=VECTOR('',#16334,1.);
#4759=VECTOR('',#16335,1.);
#4760=VECTOR('',#16336,1.);
#4761=VECTOR('',#16339,1.);
#4762=VECTOR('',#16340,1.);
#4763=VECTOR('',#16341,1.);
#4764=VECTOR('',#16344,1.);
#4765=VECTOR('',#16345,1.);
#4766=VECTOR('',#16346,1.);
#4767=VECTOR('',#16349,1.);
#4768=VECTOR('',#16350,1.);
#4769=VECTOR('',#16351,1.);
#4770=VECTOR('',#16354,1.);
#4771=VECTOR('',#16355,1.);
#4772=VECTOR('',#16356,1.);
#4773=VECTOR('',#16359,1.);
#4774=VECTOR('',#16360,1.);
#4775=VECTOR('',#16361,1.);
#4776=VECTOR('',#16364,1.);
#4777=VECTOR('',#16365,1.);
#4778=VECTOR('',#16366,1.);
#4779=VECTOR('',#16369,1.);
#4780=VECTOR('',#16370,1.);
#4781=VECTOR('',#16371,1.);
#4782=VECTOR('',#16374,1.);
#4783=VECTOR('',#16375,1.);
#4784=VECTOR('',#16376,1.);
#4785=VECTOR('',#16379,1.);
#4786=VECTOR('',#16380,1.);
#4787=VECTOR('',#16381,1.);
#4788=VECTOR('',#16384,1.);
#4789=VECTOR('',#16385,1.);
#4790=VECTOR('',#16386,1.);
#4791=VECTOR('',#16389,1.);
#4792=VECTOR('',#16390,1.);
#4793=VECTOR('',#16391,1.);
#4794=VECTOR('',#16394,1.);
#4795=VECTOR('',#16395,1.);
#4796=VECTOR('',#16396,1.);
#4797=VECTOR('',#16399,1.);
#4798=VECTOR('',#16400,1.);
#4799=VECTOR('',#16401,1.);
#4800=VECTOR('',#16404,1.);
#4801=VECTOR('',#16405,1.);
#4802=VECTOR('',#16406,1.);
#4803=VECTOR('',#16409,1.);
#4804=VECTOR('',#16410,1.);
#4805=VECTOR('',#16411,1.);
#4806=VECTOR('',#16414,1.);
#4807=VECTOR('',#16415,1.);
#4808=VECTOR('',#16416,1.);
#4809=VECTOR('',#16419,1.);
#4810=VECTOR('',#16420,1.);
#4811=VECTOR('',#16421,1.);
#4812=VECTOR('',#16424,1.);
#4813=VECTOR('',#16425,1.);
#4814=VECTOR('',#16426,1.);
#4815=VECTOR('',#16429,1.);
#4816=VECTOR('',#16430,1.);
#4817=VECTOR('',#16431,1.);
#4818=VECTOR('',#16434,1.);
#4819=VECTOR('',#16435,1.);
#4820=VECTOR('',#16436,1.);
#4821=VECTOR('',#16439,1.);
#4822=VECTOR('',#16440,1.);
#4823=VECTOR('',#16441,1.);
#4824=VECTOR('',#16444,1.);
#4825=VECTOR('',#16445,1.);
#4826=VECTOR('',#16446,1.);
#4827=VECTOR('',#16449,1.);
#4828=VECTOR('',#16450,1.);
#4829=VECTOR('',#16451,1.);
#4830=VECTOR('',#16454,1.);
#4831=VECTOR('',#16455,1.);
#4832=VECTOR('',#16456,1.);
#4833=VECTOR('',#16459,1.);
#4834=VECTOR('',#16460,1.);
#4835=VECTOR('',#16461,1.);
#4836=VECTOR('',#16464,1.);
#4837=VECTOR('',#16465,1.);
#4838=VECTOR('',#16466,1.);
#4839=VECTOR('',#16469,1.);
#4840=VECTOR('',#16470,1.);
#4841=VECTOR('',#16471,1.);
#4842=VECTOR('',#16474,1.);
#4843=VECTOR('',#16475,1.);
#4844=VECTOR('',#16476,1.);
#4845=VECTOR('',#16479,1.);
#4846=VECTOR('',#16480,1.);
#4847=VECTOR('',#16481,1.);
#4848=VECTOR('',#16484,1.);
#4849=VECTOR('',#16485,1.);
#4850=VECTOR('',#16486,1.);
#4851=VECTOR('',#16489,1.);
#4852=VECTOR('',#16490,1.);
#4853=VECTOR('',#16491,1.);
#4854=VECTOR('',#16494,1.);
#4855=VECTOR('',#16495,1.);
#4856=VECTOR('',#16496,1.);
#4857=VECTOR('',#16499,1.);
#4858=VECTOR('',#16500,1.);
#4859=VECTOR('',#16501,1.);
#4860=VECTOR('',#16504,1.);
#4861=VECTOR('',#16505,1.);
#4862=VECTOR('',#16514,1.);
#4863=VECTOR('',#16515,1.);
#4864=VECTOR('',#16528,0.5);
#4865=VECTOR('',#16537,1.2);
#4866=VECTOR('',#16548,0.164999999999999);
#4867=VECTOR('',#16551,1.);
#4868=VECTOR('',#16552,1.);
#4869=VECTOR('',#16553,1.);
#4870=VECTOR('',#16554,1.);
#4871=VECTOR('',#16557,1.);
#4872=VECTOR('',#16558,1.);
#4873=VECTOR('',#16559,1.);
#4874=VECTOR('',#16560,1.);
#4875=VECTOR('',#16563,1.);
#4876=VECTOR('',#16564,1.);
#4877=VECTOR('',#16565,1.);
#4878=VECTOR('',#16568,1.);
#4879=VECTOR('',#16569,1.);
#4880=VECTOR('',#16570,1.);
#4881=VECTOR('',#16591,1.);
#4882=VECTOR('',#16592,1.);
#4883=VECTOR('',#16593,1.);
#4884=VECTOR('',#16594,1.);
#4885=VECTOR('',#16597,1.);
#4886=VECTOR('',#16598,1.);
#4887=VECTOR('',#16599,1.);
#4888=VECTOR('',#16602,1.);
#4889=VECTOR('',#16603,1.);
#4890=VECTOR('',#16604,1.);
#4891=VECTOR('',#16607,1.);
#4892=VECTOR('',#16608,1.);
#4893=VECTOR('',#16609,1.);
#4894=VECTOR('',#16612,1.);
#4895=VECTOR('',#16613,1.);
#4896=VECTOR('',#16614,1.);
#4897=VECTOR('',#16617,1.);
#4898=VECTOR('',#16618,1.);
#4899=VECTOR('',#16629,0.185);
#4900=VECTOR('',#16634,0.2);
#4901=VECTOR('',#16639,0.1625);
#4902=VECTOR('',#16658,0.165);
#4903=VECTOR('',#16667,0.165);
#4904=VECTOR('',#16674,1.);
#4905=VECTOR('',#16675,1.);
#4906=VECTOR('',#16676,1.);
#4907=VECTOR('',#16677,1.);
#4908=VECTOR('',#16682,1.);
#4909=VECTOR('',#16683,1.);
#4910=VECTOR('',#16686,1.);
#4911=VECTOR('',#16687,1.);
#4912=VECTOR('',#16690,1.);
#4913=VECTOR('',#16691,1.);
#4914=VECTOR('',#16698,1.);
#4915=VECTOR('',#16699,1.);
#4916=VECTOR('',#16700,1.);
#4917=VECTOR('',#16701,1.);
#4918=VECTOR('',#16706,1.);
#4919=VECTOR('',#16707,1.);
#4920=VECTOR('',#16710,1.);
#4921=VECTOR('',#16711,1.);
#4922=VECTOR('',#16714,1.);
#4923=VECTOR('',#16715,1.);
#4924=VECTOR('',#16724,0.6);
#4925=VECTOR('',#16737,0.605);
#4926=VECTOR('',#16744,0.8);
#4927=VECTOR('',#16757,0.605);
#4928=VECTOR('',#16764,0.8);
#4929=VECTOR('',#16777,0.605);
#4930=VECTOR('',#16784,0.8);
#4931=VECTOR('',#16797,0.605);
#4932=VECTOR('',#16804,0.8);
#4933=VECTOR('',#16815,1.);
#4934=VECTOR('',#16816,1.);
#4935=VECTOR('',#16817,1.);
#4936=VECTOR('',#16818,1.);
#4937=VECTOR('',#16821,1.);
#4938=VECTOR('',#16822,1.);
#4939=VECTOR('',#16823,1.);
#4940=VECTOR('',#16826,1.);
#4941=VECTOR('',#16827,1.);
#4942=VECTOR('',#16828,1.);
#4943=VECTOR('',#16831,1.);
#4944=VECTOR('',#16832,1.);
#4945=VECTOR('',#16841,1.);
#4946=VECTOR('',#16842,1.);
#4947=VECTOR('',#16843,1.);
#4948=VECTOR('',#16844,1.);
#4949=VECTOR('',#16847,1.);
#4950=VECTOR('',#16848,1.);
#4951=VECTOR('',#16849,1.);
#4952=VECTOR('',#16852,1.);
#4953=VECTOR('',#16853,1.);
#4954=VECTOR('',#16854,1.);
#4955=VECTOR('',#16857,1.);
#4956=VECTOR('',#16858,1.);
#4957=VECTOR('',#16869,0.25);
#4958=VECTOR('',#16874,1.);
#4959=VECTOR('',#16875,1.);
#4960=VECTOR('',#16876,1.);
#4961=VECTOR('',#16877,1.);
#4962=VECTOR('',#16880,1.);
#4963=VECTOR('',#16881,1.);
#4964=VECTOR('',#16882,1.);
#4965=VECTOR('',#16885,1.);
#4966=VECTOR('',#16886,1.);
#4967=VECTOR('',#16887,1.);
#4968=VECTOR('',#16900,1.);
#4969=VECTOR('',#16903,1.);
#4970=VECTOR('',#16908,1.);
#4971=VECTOR('',#16909,1.);
#4972=VECTOR('',#16910,1.);
#4973=VECTOR('',#16913,1.);
#4974=VECTOR('',#16918,1.);
#4975=VECTOR('',#16919,1.);
#4976=VECTOR('',#16926,1.3);
#4977=VECTOR('',#16937,0.33);
#4978=VECTOR('',#16944,0.4);
#4979=VECTOR('',#16957,0.225);
#4980=VECTOR('',#16964,1.);
#4981=VECTOR('',#16977,0.225);
#4982=VECTOR('',#16984,1.);
#4983=VECTOR('',#16995,1.);
#4984=VECTOR('',#16996,1.);
#4985=VECTOR('',#16997,1.);
#4986=VECTOR('',#16998,1.);
#4987=VECTOR('',#17001,1.);
#4988=VECTOR('',#17002,1.);
#4989=VECTOR('',#17003,1.);
#4990=VECTOR('',#17006,1.);
#4991=VECTOR('',#17007,1.);
#4992=VECTOR('',#17008,1.);
#4993=VECTOR('',#17013,1.);
#4994=VECTOR('',#17016,1.);
#4995=VECTOR('',#17019,1.);
#4996=VECTOR('',#17022,1.);
#4997=VECTOR('',#17025,1.);
#4998=VECTOR('',#17028,1.);
#4999=VECTOR('',#17031,1.);
#5000=VECTOR('',#17034,1.);
#5001=VECTOR('',#17037,1.);
#5002=VECTOR('',#17040,1.);
#5003=VECTOR('',#17043,1.);
#5004=VECTOR('',#17046,1.);
#5005=VECTOR('',#17049,1.);
#5006=VECTOR('',#17052,1.);
#5007=VECTOR('',#17055,1.);
#5008=VECTOR('',#17058,1.);
#5009=VECTOR('',#17061,1.);
#5010=VECTOR('',#17064,1.);
#5011=VECTOR('',#17067,1.);
#5012=VECTOR('',#17070,1.);
#5013=VECTOR('',#17081,1.4);
#5014=VECTOR('',#17086,1.);
#5015=VECTOR('',#17087,1.);
#5016=VECTOR('',#17090,1.);
#5017=VECTOR('',#17091,1.);
#5018=VECTOR('',#17092,1.);
#5019=VECTOR('',#17097,1.);
#5020=VECTOR('',#17098,1.);
#5021=VECTOR('',#17101,1.);
#5022=VECTOR('',#17102,1.);
#5023=VECTOR('',#17103,1.);
#5024=VECTOR('',#17108,1.);
#5025=VECTOR('',#17109,1.);
#5026=VECTOR('',#17112,1.);
#5027=VECTOR('',#17113,1.);
#5028=VECTOR('',#17114,1.);
#5029=VECTOR('',#17119,1.);
#5030=VECTOR('',#17120,1.);
#5031=VECTOR('',#17123,1.);
#5032=VECTOR('',#17124,1.);
#5033=VECTOR('',#17125,1.);
#5034=VECTOR('',#17130,1.);
#5035=VECTOR('',#17131,1.);
#5036=VECTOR('',#17134,1.);
#5037=VECTOR('',#17135,1.);
#5038=VECTOR('',#17136,1.);
#5039=VECTOR('',#17141,1.);
#5040=VECTOR('',#17142,1.);
#5041=VECTOR('',#17145,1.);
#5042=VECTOR('',#17146,1.);
#5043=VECTOR('',#17147,1.);
#5044=VECTOR('',#17152,1.);
#5045=VECTOR('',#17153,1.);
#5046=VECTOR('',#17156,1.);
#5047=VECTOR('',#17157,1.);
#5048=VECTOR('',#17158,1.);
#5049=VECTOR('',#17163,1.);
#5050=VECTOR('',#17164,1.);
#5051=VECTOR('',#17167,1.);
#5052=VECTOR('',#17168,1.);
#5053=VECTOR('',#17169,1.);
#5054=VECTOR('',#17174,1.);
#5055=VECTOR('',#17175,1.);
#5056=VECTOR('',#17178,1.);
#5057=VECTOR('',#17179,1.);
#5058=VECTOR('',#17180,1.);
#5059=VECTOR('',#17185,1.);
#5060=VECTOR('',#17186,1.);
#5061=VECTOR('',#17189,1.);
#5062=VECTOR('',#17190,1.);
#5063=VECTOR('',#17191,1.);
#5064=VECTOR('',#17196,1.);
#5065=VECTOR('',#17197,1.);
#5066=VECTOR('',#17200,1.);
#5067=VECTOR('',#17201,1.);
#5068=VECTOR('',#17202,1.);
#5069=VECTOR('',#17207,1.);
#5070=VECTOR('',#17208,1.);
#5071=VECTOR('',#17211,1.);
#5072=VECTOR('',#17212,1.);
#5073=VECTOR('',#17213,1.);
#5074=VECTOR('',#17218,1.);
#5075=VECTOR('',#17219,1.);
#5076=VECTOR('',#17222,1.);
#5077=VECTOR('',#17223,1.);
#5078=VECTOR('',#17224,1.);
#5079=VECTOR('',#17229,1.);
#5080=VECTOR('',#17230,1.);
#5081=VECTOR('',#17233,1.);
#5082=VECTOR('',#17234,1.);
#5083=VECTOR('',#17235,1.);
#5084=VECTOR('',#17240,1.);
#5085=VECTOR('',#17241,1.);
#5086=VECTOR('',#17244,1.);
#5087=VECTOR('',#17245,1.);
#5088=VECTOR('',#17246,1.);
#5089=VECTOR('',#17251,1.);
#5090=VECTOR('',#17252,1.);
#5091=VECTOR('',#17255,1.);
#5092=VECTOR('',#17256,1.);
#5093=VECTOR('',#17257,1.);
#5094=VECTOR('',#17262,1.);
#5095=VECTOR('',#17263,1.);
#5096=VECTOR('',#17266,1.);
#5097=VECTOR('',#17267,1.);
#5098=VECTOR('',#17268,1.);
#5099=VECTOR('',#17273,1.);
#5100=VECTOR('',#17274,1.);
#5101=VECTOR('',#17277,1.);
#5102=VECTOR('',#17278,1.);
#5103=VECTOR('',#17279,1.);
#5104=VECTOR('',#17284,1.);
#5105=VECTOR('',#17285,1.);
#5106=VECTOR('',#17288,1.);
#5107=VECTOR('',#17289,1.);
#5108=VECTOR('',#17290,1.);
#5109=VECTOR('',#17295,1.);
#5110=VECTOR('',#17296,1.);
#5111=VECTOR('',#17299,1.);
#5112=VECTOR('',#17300,1.);
#5113=VECTOR('',#17301,1.);
#5114=VECTOR('',#17314,0.32);
#5115=VECTOR('',#17321,0.6);
#5116=VECTOR('',#17338,0.475);
#5117=VECTOR('',#17343,0.5);
#5118=VECTOR('',#17348,0.485);
#5119=VECTOR('',#17357,0.31);
#5120=VECTOR('',#17362,0.3);
#5121=VECTOR('',#17367,0.27);
#5122=VECTOR('',#17372,1.);
#5123=VECTOR('',#17373,1.);
#5124=VECTOR('',#17374,1.);
#5125=VECTOR('',#17375,1.);
#5126=VECTOR('',#17378,1.);
#5127=VECTOR('',#17379,1.);
#5128=VECTOR('',#17380,1.);
#5129=VECTOR('',#17383,1.);
#5130=VECTOR('',#17384,1.);
#5131=VECTOR('',#17385,1.);
#5132=VECTOR('',#17388,1.);
#5133=VECTOR('',#17389,1.);
#5134=VECTOR('',#17390,1.);
#5135=VECTOR('',#17393,1.);
#5136=VECTOR('',#17394,1.);
#5137=VECTOR('',#17395,1.);
#5138=VECTOR('',#17398,1.);
#5139=VECTOR('',#17399,1.);
#5140=VECTOR('',#17414,0.325);
#5141=VECTOR('',#17419,0.35);
#5142=VECTOR('',#17424,0.335);
#5143=VECTOR('',#17433,0.21);
#5144=VECTOR('',#17438,0.2);
#5145=VECTOR('',#17443,0.18);
#5146=VECTOR('',#17448,1.);
#5147=VECTOR('',#17449,1.);
#5148=VECTOR('',#17450,1.);
#5149=VECTOR('',#17451,1.);
#5150=VECTOR('',#17454,1.);
#5151=VECTOR('',#17455,1.);
#5152=VECTOR('',#17456,1.);
#5153=VECTOR('',#17459,1.);
#5154=VECTOR('',#17460,1.);
#5155=VECTOR('',#17461,1.);
#5156=VECTOR('',#17464,1.);
#5157=VECTOR('',#17465,1.);
#5158=VECTOR('',#17466,1.);
#5159=VECTOR('',#17469,1.);
#5160=VECTOR('',#17470,1.);
#5161=VECTOR('',#17471,1.);
#5162=VECTOR('',#17474,1.);
#5163=VECTOR('',#17475,1.);
#5164=VECTOR('',#17614,0.405);
#5165=VECTOR('',#17621,0.9);
#5166=CIRCLE('',#13003,0.165);
#5167=CIRCLE('',#13004,0.165);
#5168=CIRCLE('',#13006,0.165);
#5169=CIRCLE('',#13007,0.165);
#5170=CIRCLE('',#13009,0.165);
#5171=CIRCLE('',#13010,0.165);
#5172=CIRCLE('',#13012,0.165);
#5173=CIRCLE('',#13013,0.165);
#5174=CIRCLE('',#13015,0.165);
#5175=CIRCLE('',#13016,0.165);
#5176=CIRCLE('',#13018,0.165);
#5177=CIRCLE('',#13019,0.165);
#5178=CIRCLE('',#13021,0.21);
#5179=CIRCLE('',#13022,0.21);
#5180=CIRCLE('',#13024,0.21);
#5181=CIRCLE('',#13025,0.21);
#5182=CIRCLE('',#13027,0.21);
#5183=CIRCLE('',#13028,0.21);
#5184=CIRCLE('',#13030,0.21);
#5185=CIRCLE('',#13031,0.21);
#5186=CIRCLE('',#13054,0.165);
#5187=CIRCLE('',#13055,0.165);
#5188=CIRCLE('',#13058,0.165);
#5189=CIRCLE('',#13059,0.165);
#5190=CIRCLE('',#13064,2.);
#5191=CIRCLE('',#13065,2.);
#5192=CIRCLE('',#13066,1.4);
#5193=CIRCLE('',#13068,1.4);
#5194=CIRCLE('',#13070,2.);
#5195=CIRCLE('',#13072,2.);
#5196=CIRCLE('',#13077,0.165);
#5197=CIRCLE('',#13078,0.165);
#5198=CIRCLE('',#13081,0.165);
#5199=CIRCLE('',#13082,0.165);
#5200=CIRCLE('',#13087,2.);
#5201=CIRCLE('',#13088,2.);
#5202=CIRCLE('',#13089,1.4);
#5203=CIRCLE('',#13091,1.4);
#5204=CIRCLE('',#13093,2.);
#5205=CIRCLE('',#13095,2.);
#5206=CIRCLE('',#13100,0.275);
#5207=CIRCLE('',#13101,0.275);
#5208=CIRCLE('',#13103,0.275);
#5209=CIRCLE('',#13104,0.275);
#5210=CIRCLE('',#13106,0.275);
#5211=CIRCLE('',#13107,0.275);
#5212=CIRCLE('',#13109,0.275);
#5213=CIRCLE('',#13110,0.275);
#5214=CIRCLE('',#13128,1.4);
#5215=CIRCLE('',#13129,1.005);
#5216=CIRCLE('',#13131,1.005);
#5217=CIRCLE('',#13133,1.4);
#5218=CIRCLE('',#13135,1.6);
#5219=CIRCLE('',#13137,1.6);
#5220=CIRCLE('',#13141,0.225);
#5221=CIRCLE('',#13142,0.225);
#5222=CIRCLE('',#13144,0.225);
#5223=CIRCLE('',#13145,0.225);
#5224=CIRCLE('',#13153,1.01);
#5225=CIRCLE('',#13155,1.01);
#5226=CIRCLE('',#13166,1.4);
#5227=CIRCLE('',#13167,1.005);
#5228=CIRCLE('',#13169,1.005);
#5229=CIRCLE('',#13171,1.4);
#5230=CIRCLE('',#13173,1.6);
#5231=CIRCLE('',#13175,1.6);
#5232=CIRCLE('',#13179,0.225);
#5233=CIRCLE('',#13180,0.225);
#5234=CIRCLE('',#13182,0.225);
#5235=CIRCLE('',#13183,0.225);
#5236=CIRCLE('',#13191,1.01);
#5237=CIRCLE('',#13193,1.01);
#5238=CIRCLE('',#13200,0.4);
#5239=CIRCLE('',#13201,0.4);
#5240=CIRCLE('',#13203,0.225);
#5241=CIRCLE('',#13205,0.4);
#5242=CIRCLE('',#13206,0.4);
#5243=CIRCLE('',#13208,0.225);
#5244=CIRCLE('',#13210,0.225);
#5245=CIRCLE('',#13212,0.225);
#5246=CIRCLE('',#13214,2.5);
#5247=CIRCLE('',#13215,2.5);
#5248=CIRCLE('',#13220,2.52);
#5249=CIRCLE('',#13221,2.52);
#5250=CIRCLE('',#13223,0.225);
#5251=CIRCLE('',#13224,0.225);
#5252=CIRCLE('',#13227,0.165);
#5253=CIRCLE('',#13228,0.165);
#5254=CIRCLE('',#13230,0.165);
#5255=CIRCLE('',#13231,0.165);
#5256=CIRCLE('',#13233,0.165);
#5257=CIRCLE('',#13234,0.165);
#5258=CIRCLE('',#13236,0.165);
#5259=CIRCLE('',#13237,0.165);
#5260=CIRCLE('',#13239,0.225);
#5261=CIRCLE('',#13241,0.225);
#5262=CIRCLE('',#13243,1.6);
#5263=CIRCLE('',#13244,1.6);
#5264=CIRCLE('',#13255,1.41);
#5265=CIRCLE('',#13256,1.41);
#5266=CIRCLE('',#13258,0.225);
#5267=CIRCLE('',#13259,0.225);
#5268=CIRCLE('',#13261,0.225);
#5269=CIRCLE('',#13262,0.225);
#5270=CIRCLE('',#13264,0.225);
#5271=CIRCLE('',#13265,0.225);
#5272=CIRCLE('',#13267,0.225);
#5273=CIRCLE('',#13268,0.225);
#5274=CIRCLE('',#13270,1.59);
#5275=CIRCLE('',#13271,1.59);
#5276=CIRCLE('',#13274,2.4);
#5277=CIRCLE('',#13275,2.4);
#5278=CIRCLE('',#13280,1.41);
#5279=CIRCLE('',#13281,1.41);
#5280=CIRCLE('',#13283,0.225);
#5281=CIRCLE('',#13284,0.225);
#5282=CIRCLE('',#13286,0.225);
#5283=CIRCLE('',#13287,0.225);
#5284=CIRCLE('',#13289,0.225);
#5285=CIRCLE('',#13290,0.225);
#5286=CIRCLE('',#13292,0.225);
#5287=CIRCLE('',#13293,0.225);
#5288=CIRCLE('',#13295,1.59);
#5289=CIRCLE('',#13296,1.59);
#5290=CIRCLE('',#13299,2.4);
#5291=CIRCLE('',#13300,2.4);
#5292=CIRCLE('',#13305,2.52);
#5293=CIRCLE('',#13306,2.52);
#5294=CIRCLE('',#13308,0.225);
#5295=CIRCLE('',#13309,0.225);
#5296=CIRCLE('',#13311,0.165);
#5297=CIRCLE('',#13312,0.165);
#5298=CIRCLE('',#13313,0.165);
#5299=CIRCLE('',#13314,0.165);
#5300=CIRCLE('',#13315,1.6);
#5301=CIRCLE('',#13317,0.165);
#5302=CIRCLE('',#13319,0.165);
#5303=CIRCLE('',#13321,0.165);
#5304=CIRCLE('',#13323,0.165);
#5305=CIRCLE('',#13325,0.225);
#5306=CIRCLE('',#13327,0.225);
#5307=CIRCLE('',#13329,1.6);
#5308=CIRCLE('',#13340,1.41);
#5309=CIRCLE('',#13341,1.41);
#5310=CIRCLE('',#13343,0.225);
#5311=CIRCLE('',#13344,0.225);
#5312=CIRCLE('',#13346,0.225);
#5313=CIRCLE('',#13347,0.225);
#5314=CIRCLE('',#13349,0.225);
#5315=CIRCLE('',#13350,0.225);
#5316=CIRCLE('',#13352,0.225);
#5317=CIRCLE('',#13353,0.225);
#5318=CIRCLE('',#13355,1.59);
#5319=CIRCLE('',#13356,1.59);
#5320=CIRCLE('',#13359,2.4);
#5321=CIRCLE('',#13360,2.4);
#5322=CIRCLE('',#13365,1.41);
#5323=CIRCLE('',#13366,1.41);
#5324=CIRCLE('',#13368,0.225);
#5325=CIRCLE('',#13369,0.225);
#5326=CIRCLE('',#13371,0.225);
#5327=CIRCLE('',#13372,0.225);
#5328=CIRCLE('',#13374,0.225);
#5329=CIRCLE('',#13375,0.225);
#5330=CIRCLE('',#13377,0.225);
#5331=CIRCLE('',#13378,0.225);
#5332=CIRCLE('',#13380,1.59);
#5333=CIRCLE('',#13381,1.59);
#5334=CIRCLE('',#13384,2.4);
#5335=CIRCLE('',#13385,2.4);
#5336=CIRCLE('',#13390,0.375);
#5337=CIRCLE('',#13392,0.425);
#5338=CIRCLE('',#13394,0.425);
#5339=CIRCLE('',#13396,0.395);
#5340=CIRCLE('',#13398,0.27);
#5341=CIRCLE('',#13400,0.24505);
#5342=CIRCLE('',#13402,0.24505);
#5343=CIRCLE('',#13404,0.2);
#5344=CIRCLE('',#13417,1.070235);
#5345=CIRCLE('',#13418,1.070235);
#5346=CIRCLE('',#13419,0.309556);
#5347=CIRCLE('',#13420,1.070235);
#5348=CIRCLE('',#13421,1.070235);
#5349=CIRCLE('',#13423,1.070235);
#5350=CIRCLE('',#13425,0.6);
#5351=CIRCLE('',#13426,0.6);
#5352=CIRCLE('',#13428,0.66);
#5353=CIRCLE('',#13431,1.070235);
#5354=CIRCLE('',#13433,0.66);
#5355=CIRCLE('',#13437,1.129765);
#5356=CIRCLE('',#13438,1.129765);
#5357=CIRCLE('',#13439,0.309556);
#5358=CIRCLE('',#13440,1.129765);
#5359=CIRCLE('',#13441,1.129765);
#5360=CIRCLE('',#13443,1.129765);
#5361=CIRCLE('',#13445,1.54);
#5362=CIRCLE('',#13446,1.129765);
#5363=CIRCLE('',#13448,1.6);
#5364=CIRCLE('',#13450,1.6);
#5365=CIRCLE('',#13452,1.54);
#5366=CIRCLE('',#13457,0.29765);
#5367=CIRCLE('',#13459,0.29765);
#5368=CIRCLE('',#13461,0.29765);
#5369=CIRCLE('',#13463,0.29765);
#5370=CIRCLE('',#13465,0.29765);
#5371=CIRCLE('',#13467,0.29765);
#5372=CIRCLE('',#13469,0.29765);
#5373=CIRCLE('',#13472,0.303778037777585);
#5374=CIRCLE('',#13473,0.303778037777585);
#5375=CIRCLE('',#13475,1.123812);
#5376=CIRCLE('',#13476,1.123812);
#5377=CIRCLE('',#13477,1.123812);
#5378=CIRCLE('',#13478,1.123812);
#5379=CIRCLE('',#13479,1.123812);
#5380=CIRCLE('',#13480,1.123812);
#5381=CIRCLE('',#13481,1.123812);
#5382=CIRCLE('',#13482,1.123812);
#5383=CIRCLE('',#13483,1.123812);
#5384=CIRCLE('',#13485,1.076188);
#5385=CIRCLE('',#13486,0.303778037777585);
#5386=CIRCLE('',#13488,0.303778037777585);
#5387=CIRCLE('',#13490,1.076188);
#5388=CIRCLE('',#13491,0.303778037777585);
#5389=CIRCLE('',#13493,0.303778037777585);
#5390=CIRCLE('',#13495,1.076188);
#5391=CIRCLE('',#13496,1.076188);
#5392=CIRCLE('',#13497,0.303778037777585);
#5393=CIRCLE('',#13499,0.303778037777585);
#5394=CIRCLE('',#13501,1.076188);
#5395=CIRCLE('',#13502,0.303778037777585);
#5396=CIRCLE('',#13504,0.303778037777585);
#5397=CIRCLE('',#13506,1.076188);
#5398=CIRCLE('',#13507,0.303778037777585);
#5399=CIRCLE('',#13509,0.303778037777585);
#5400=CIRCLE('',#13511,1.076188);
#5401=CIRCLE('',#13512,1.076188);
#5402=CIRCLE('',#13513,1.076188);
#5403=CIRCLE('',#13515,0.303778037777585);
#5404=CIRCLE('',#13517,0.303778037777585);
#5405=CIRCLE('',#13522,1.119765);
#5406=CIRCLE('',#13523,1.085235);
#5407=CIRCLE('',#13525,1.119765);
#5408=CIRCLE('',#13527,1.085235);
#5409=CIRCLE('',#13530,1.119765);
#5410=CIRCLE('',#13531,1.085235);
#5411=CIRCLE('',#13533,1.119765);
#5412=CIRCLE('',#13535,1.085235);
#5413=CIRCLE('',#13552,0.1954);
#5414=CIRCLE('',#13554,0.3);
#5415=CIRCLE('',#13556,0.35);
#5416=CIRCLE('',#13558,0.35);
#5417=CIRCLE('',#13560,0.32);
#5418=CIRCLE('',#13562,0.22);
#5419=CIRCLE('',#13564,0.1954);
#5420=CIRCLE('',#13569,0.425);
#5421=CIRCLE('',#13570,0.425);
#5422=CIRCLE('',#13575,1.);
#5423=CIRCLE('',#13576,1.);
#5424=CIRCLE('',#13578,1.);
#5425=CIRCLE('',#13579,1.);
#5426=CIRCLE('',#13744,1.);
#5427=CIRCLE('',#13745,1.);
#5428=CIRCLE('',#13750,0.5);
#5429=CIRCLE('',#13751,0.5);
#5430=CIRCLE('',#13754,1.2);
#5431=CIRCLE('',#13755,1.2);
#5432=CIRCLE('',#13765,1.005);
#5433=CIRCLE('',#13766,1.7);
#5434=CIRCLE('',#13768,1.7);
#5435=CIRCLE('',#13770,1.005);
#5436=CIRCLE('',#13781,0.17);
#5437=CIRCLE('',#13783,0.1954);
#5438=CIRCLE('',#13785,0.1954);
#5439=CIRCLE('',#13787,0.125);
#5440=CIRCLE('',#13796,0.165);
#5441=CIRCLE('',#13797,0.165);
#5442=CIRCLE('',#13800,0.165);
#5443=CIRCLE('',#13801,0.165);
#5444=CIRCLE('',#13805,0.6);
#5445=CIRCLE('',#13809,0.6);
#5446=CIRCLE('',#13812,0.6);
#5447=CIRCLE('',#13816,0.6);
#5448=CIRCLE('',#13818,0.6);
#5449=CIRCLE('',#13819,0.6);
#5450=CIRCLE('',#13824,0.605);
#5451=CIRCLE('',#13825,0.605);
#5452=CIRCLE('',#13827,0.8);
#5453=CIRCLE('',#13828,0.8);
#5454=CIRCLE('',#13833,0.605);
#5455=CIRCLE('',#13834,0.605);
#5456=CIRCLE('',#13836,0.8);
#5457=CIRCLE('',#13837,0.8);
#5458=CIRCLE('',#13842,0.605);
#5459=CIRCLE('',#13843,0.605);
#5460=CIRCLE('',#13845,0.8);
#5461=CIRCLE('',#13846,0.8);
#5462=CIRCLE('',#13851,0.605);
#5463=CIRCLE('',#13852,0.605);
#5464=CIRCLE('',#13854,0.8);
#5465=CIRCLE('',#13855,0.8);
#5466=CIRCLE('',#13874,0.25);
#5467=CIRCLE('',#13875,0.25);
#5468=CIRCLE('',#13880,1.3);
#5469=CIRCLE('',#13881,0.6);
#5470=CIRCLE('',#13883,0.6);
#5471=CIRCLE('',#13885,0.9);
#5472=CIRCLE('',#13886,0.9);
#5473=CIRCLE('',#13889,1.3);
#5474=CIRCLE('',#13892,1.3);
#5475=CIRCLE('',#13894,1.3);
#5476=CIRCLE('',#13898,0.33);
#5477=CIRCLE('',#13899,0.33);
#5478=CIRCLE('',#13901,0.4);
#5479=CIRCLE('',#13902,0.4);
#5480=CIRCLE('',#13907,0.225);
#5481=CIRCLE('',#13908,0.225);
#5482=CIRCLE('',#13910,1.);
#5483=CIRCLE('',#13911,1.);
#5484=CIRCLE('',#13916,0.225);
#5485=CIRCLE('',#13917,0.225);
#5486=CIRCLE('',#13919,1.);
#5487=CIRCLE('',#13920,1.);
#5488=CIRCLE('',#13928,1.75);
#5489=CIRCLE('',#13929,1.75);
#5490=CIRCLE('',#13930,1.75);
#5491=CIRCLE('',#13931,1.75);
#5492=CIRCLE('',#13932,1.75);
#5493=CIRCLE('',#13933,1.75);
#5494=CIRCLE('',#13934,1.75);
#5495=CIRCLE('',#13935,1.75);
#5496=CIRCLE('',#13936,1.75);
#5497=CIRCLE('',#13937,1.75);
#5498=CIRCLE('',#13938,1.75);
#5499=CIRCLE('',#13939,1.75);
#5500=CIRCLE('',#13940,1.75);
#5501=CIRCLE('',#13941,1.75);
#5502=CIRCLE('',#13942,1.75);
#5503=CIRCLE('',#13943,1.75);
#5504=CIRCLE('',#13944,1.75);
#5505=CIRCLE('',#13945,1.75);
#5506=CIRCLE('',#13946,1.75);
#5507=CIRCLE('',#13947,1.75);
#5508=CIRCLE('',#13948,0.6);
#5509=CIRCLE('',#13950,0.6);
#5510=CIRCLE('',#13952,1.4);
#5511=CIRCLE('',#13953,1.4);
#5512=CIRCLE('',#13957,1.75);
#5513=CIRCLE('',#13960,1.75);
#5514=CIRCLE('',#13963,1.75);
#5515=CIRCLE('',#13966,1.75);
#5516=CIRCLE('',#13969,1.75);
#5517=CIRCLE('',#13972,1.75);
#5518=CIRCLE('',#13975,1.75);
#5519=CIRCLE('',#13978,1.75);
#5520=CIRCLE('',#13981,1.75);
#5521=CIRCLE('',#13984,1.75);
#5522=CIRCLE('',#13987,1.75);
#5523=CIRCLE('',#13990,1.75);
#5524=CIRCLE('',#13993,1.75);
#5525=CIRCLE('',#13996,1.75);
#5526=CIRCLE('',#13999,1.75);
#5527=CIRCLE('',#14002,1.75);
#5528=CIRCLE('',#14005,1.75);
#5529=CIRCLE('',#14008,1.75);
#5530=CIRCLE('',#14011,1.75);
#5531=CIRCLE('',#14014,1.75);
#5532=CIRCLE('',#14018,0.32);
#5533=CIRCLE('',#14019,0.32);
#5534=CIRCLE('',#14021,0.6);
#5535=CIRCLE('',#14022,0.6);
#5536=CIRCLE('',#14027,0.45);
#5537=CIRCLE('',#14029,0.5);
#5538=CIRCLE('',#14031,0.5);
#5539=CIRCLE('',#14033,0.47);
#5540=CIRCLE('',#14035,0.32);
#5541=CIRCLE('',#14037,0.2942);
#5542=CIRCLE('',#14039,0.2942);
#5543=CIRCLE('',#14041,0.24);
#5544=CIRCLE('',#14053,0.3);
#5545=CIRCLE('',#14055,0.35);
#5546=CIRCLE('',#14057,0.35);
#5547=CIRCLE('',#14059,0.32);
#5548=CIRCLE('',#14061,0.22);
#5549=CIRCLE('',#14063,0.1954);
#5550=CIRCLE('',#14065,0.1954);
#5551=CIRCLE('',#14067,0.16);
#5552=CIRCLE('',#14143,0.405);
#5553=CIRCLE('',#14144,0.405);
#5554=CIRCLE('',#14146,0.9);
#5555=CIRCLE('',#14147,0.9);
#5556=VERTEX_POINT('',#17642);
#5557=VERTEX_POINT('',#17644);
#5558=VERTEX_POINT('',#17648);
#5559=VERTEX_POINT('',#17650);
#5560=VERTEX_POINT('',#17654);
#5561=VERTEX_POINT('',#17656);
#5562=VERTEX_POINT('',#17660);
#5563=VERTEX_POINT('',#17662);
#5564=VERTEX_POINT('',#17666);
#5565=VERTEX_POINT('',#17668);
#5566=VERTEX_POINT('',#17672);
#5567=VERTEX_POINT('',#17674);
#5568=VERTEX_POINT('',#17678);
#5569=VERTEX_POINT('',#17680);
#5570=VERTEX_POINT('',#17684);
#5571=VERTEX_POINT('',#17686);
#5572=VERTEX_POINT('',#17690);
#5573=VERTEX_POINT('',#17692);
#5574=VERTEX_POINT('',#17696);
#5575=VERTEX_POINT('',#17698);
#5576=VERTEX_POINT('',#17702);
#5577=VERTEX_POINT('',#17703);
#5578=VERTEX_POINT('',#17705);
#5579=VERTEX_POINT('',#17707);
#5580=VERTEX_POINT('',#17711);
#5581=VERTEX_POINT('',#17713);
#5582=VERTEX_POINT('',#17717);
#5583=VERTEX_POINT('',#17719);
#5584=VERTEX_POINT('',#17729);
#5585=VERTEX_POINT('',#17730);
#5586=VERTEX_POINT('',#17732);
#5587=VERTEX_POINT('',#17734);
#5588=VERTEX_POINT('',#17738);
#5589=VERTEX_POINT('',#17740);
#5590=VERTEX_POINT('',#17744);
#5591=VERTEX_POINT('',#17746);
#5592=VERTEX_POINT('',#17756);
#5593=VERTEX_POINT('',#17757);
#5594=VERTEX_POINT('',#17759);
#5595=VERTEX_POINT('',#17761);
#5596=VERTEX_POINT('',#17765);
#5597=VERTEX_POINT('',#17767);
#5598=VERTEX_POINT('',#17771);
#5599=VERTEX_POINT('',#17773);
#5600=VERTEX_POINT('',#17783);
#5601=VERTEX_POINT('',#17785);
#5602=VERTEX_POINT('',#17790);
#5603=VERTEX_POINT('',#17792);
#5604=VERTEX_POINT('',#17797);
#5605=VERTEX_POINT('',#17798);
#5606=VERTEX_POINT('',#17800);
#5607=VERTEX_POINT('',#17802);
#5608=VERTEX_POINT('',#17806);
#5609=VERTEX_POINT('',#17807);
#5610=VERTEX_POINT('',#17809);
#5611=VERTEX_POINT('',#17811);
#5612=VERTEX_POINT('',#17815);
#5613=VERTEX_POINT('',#17817);
#5614=VERTEX_POINT('',#17819);
#5615=VERTEX_POINT('',#17821);
#5616=VERTEX_POINT('',#17828);
#5617=VERTEX_POINT('',#17832);
#5618=VERTEX_POINT('',#17836);
#5619=VERTEX_POINT('',#17838);
#5620=VERTEX_POINT('',#17846);
#5621=VERTEX_POINT('',#17848);
#5622=VERTEX_POINT('',#17853);
#5623=VERTEX_POINT('',#17855);
#5624=VERTEX_POINT('',#17860);
#5625=VERTEX_POINT('',#17861);
#5626=VERTEX_POINT('',#17863);
#5627=VERTEX_POINT('',#17865);
#5628=VERTEX_POINT('',#17869);
#5629=VERTEX_POINT('',#17870);
#5630=VERTEX_POINT('',#17872);
#5631=VERTEX_POINT('',#17874);
#5632=VERTEX_POINT('',#17878);
#5633=VERTEX_POINT('',#17880);
#5634=VERTEX_POINT('',#17882);
#5635=VERTEX_POINT('',#17884);
#5636=VERTEX_POINT('',#17891);
#5637=VERTEX_POINT('',#17895);
#5638=VERTEX_POINT('',#17899);
#5639=VERTEX_POINT('',#17901);
#5640=VERTEX_POINT('',#17909);
#5641=VERTEX_POINT('',#17911);
#5642=VERTEX_POINT('',#17915);
#5643=VERTEX_POINT('',#17917);
#5644=VERTEX_POINT('',#17921);
#5645=VERTEX_POINT('',#17923);
#5646=VERTEX_POINT('',#17927);
#5647=VERTEX_POINT('',#17929);
#5648=VERTEX_POINT('',#17933);
#5649=VERTEX_POINT('',#17934);
#5650=VERTEX_POINT('',#17936);
#5651=VERTEX_POINT('',#17938);
#5652=VERTEX_POINT('',#17941);
#5653=VERTEX_POINT('',#17942);
#5654=VERTEX_POINT('',#17944);
#5655=VERTEX_POINT('',#17946);
#5656=VERTEX_POINT('',#17950);
#5657=VERTEX_POINT('',#17951);
#5658=VERTEX_POINT('',#17956);
#5659=VERTEX_POINT('',#17960);
#5660=VERTEX_POINT('',#17966);
#5661=VERTEX_POINT('',#17968);
#5662=VERTEX_POINT('',#17972);
#5663=VERTEX_POINT('',#17976);
#5664=VERTEX_POINT('',#17985);
#5665=VERTEX_POINT('',#17986);
#5666=VERTEX_POINT('',#17988);
#5667=VERTEX_POINT('',#17990);
#5668=VERTEX_POINT('',#17994);
#5669=VERTEX_POINT('',#17995);
#5670=VERTEX_POINT('',#17997);
#5671=VERTEX_POINT('',#17999);
#5672=VERTEX_POINT('',#18003);
#5673=VERTEX_POINT('',#18005);
#5674=VERTEX_POINT('',#18007);
#5675=VERTEX_POINT('',#18009);
#5676=VERTEX_POINT('',#18013);
#5677=VERTEX_POINT('',#18015);
#5678=VERTEX_POINT('',#18017);
#5679=VERTEX_POINT('',#18019);
#5680=VERTEX_POINT('',#18036);
#5681=VERTEX_POINT('',#18038);
#5682=VERTEX_POINT('',#18042);
#5683=VERTEX_POINT('',#18044);
#5684=VERTEX_POINT('',#18048);
#5685=VERTEX_POINT('',#18049);
#5686=VERTEX_POINT('',#18051);
#5687=VERTEX_POINT('',#18053);
#5688=VERTEX_POINT('',#18057);
#5689=VERTEX_POINT('',#18058);
#5690=VERTEX_POINT('',#18060);
#5691=VERTEX_POINT('',#18062);
#5692=VERTEX_POINT('',#18066);
#5693=VERTEX_POINT('',#18068);
#5694=VERTEX_POINT('',#18072);
#5695=VERTEX_POINT('',#18074);
#5696=VERTEX_POINT('',#18078);
#5697=VERTEX_POINT('',#18080);
#5698=VERTEX_POINT('',#18084);
#5699=VERTEX_POINT('',#18086);
#5700=VERTEX_POINT('',#18091);
#5701=VERTEX_POINT('',#18093);
#5702=VERTEX_POINT('',#18099);
#5703=VERTEX_POINT('',#18103);
#5704=VERTEX_POINT('',#18111);
#5705=VERTEX_POINT('',#18112);
#5706=VERTEX_POINT('',#18114);
#5707=VERTEX_POINT('',#18116);
#5708=VERTEX_POINT('',#18120);
#5709=VERTEX_POINT('',#18121);
#5710=VERTEX_POINT('',#18123);
#5711=VERTEX_POINT('',#18125);
#5712=VERTEX_POINT('',#18129);
#5713=VERTEX_POINT('',#18131);
#5714=VERTEX_POINT('',#18133);
#5715=VERTEX_POINT('',#18135);
#5716=VERTEX_POINT('',#18139);
#5717=VERTEX_POINT('',#18141);
#5718=VERTEX_POINT('',#18143);
#5719=VERTEX_POINT('',#18145);
#5720=VERTEX_POINT('',#18162);
#5721=VERTEX_POINT('',#18164);
#5722=VERTEX_POINT('',#18168);
#5723=VERTEX_POINT('',#18170);
#5724=VERTEX_POINT('',#18174);
#5725=VERTEX_POINT('',#18175);
#5726=VERTEX_POINT('',#18177);
#5727=VERTEX_POINT('',#18179);
#5728=VERTEX_POINT('',#18183);
#5729=VERTEX_POINT('',#18184);
#5730=VERTEX_POINT('',#18186);
#5731=VERTEX_POINT('',#18188);
#5732=VERTEX_POINT('',#18192);
#5733=VERTEX_POINT('',#18194);
#5734=VERTEX_POINT('',#18198);
#5735=VERTEX_POINT('',#18200);
#5736=VERTEX_POINT('',#18204);
#5737=VERTEX_POINT('',#18206);
#5738=VERTEX_POINT('',#18210);
#5739=VERTEX_POINT('',#18212);
#5740=VERTEX_POINT('',#18217);
#5741=VERTEX_POINT('',#18219);
#5742=VERTEX_POINT('',#18225);
#5743=VERTEX_POINT('',#18229);
#5744=VERTEX_POINT('',#18237);
#5745=VERTEX_POINT('',#18239);
#5746=VERTEX_POINT('',#18243);
#5747=VERTEX_POINT('',#18246);
#5748=VERTEX_POINT('',#18248);
#5749=VERTEX_POINT('',#18252);
#5750=VERTEX_POINT('',#18255);
#5751=VERTEX_POINT('',#18259);
#5752=VERTEX_POINT('',#18263);
#5753=VERTEX_POINT('',#18265);
#5754=VERTEX_POINT('',#18272);
#5755=VERTEX_POINT('',#18273);
#5756=VERTEX_POINT('',#18275);
#5757=VERTEX_POINT('',#18277);
#5758=VERTEX_POINT('',#18281);
#5759=VERTEX_POINT('',#18283);
#5760=VERTEX_POINT('',#18285);
#5761=VERTEX_POINT('',#18288);
#5762=VERTEX_POINT('',#18290);
#5763=VERTEX_POINT('',#18293);
#5764=VERTEX_POINT('',#18297);
#5765=VERTEX_POINT('',#18299);
#5766=VERTEX_POINT('',#18303);
#5767=VERTEX_POINT('',#18305);
#5768=VERTEX_POINT('',#18309);
#5769=VERTEX_POINT('',#18311);
#5770=VERTEX_POINT('',#18315);
#5771=VERTEX_POINT('',#18317);
#5772=VERTEX_POINT('',#18321);
#5773=VERTEX_POINT('',#18325);
#5774=VERTEX_POINT('',#18329);
#5775=VERTEX_POINT('',#18331);
#5776=VERTEX_POINT('',#18335);
#5777=VERTEX_POINT('',#18337);
#5778=VERTEX_POINT('',#18341);
#5779=VERTEX_POINT('',#18342);
#5780=VERTEX_POINT('',#18344);
#5781=VERTEX_POINT('',#18346);
#5782=VERTEX_POINT('',#18353);
#5783=VERTEX_POINT('',#18355);
#5784=VERTEX_POINT('',#18359);
#5785=VERTEX_POINT('',#18363);
#5786=VERTEX_POINT('',#18371);
#5787=VERTEX_POINT('',#18373);
#5788=VERTEX_POINT('',#18377);
#5789=VERTEX_POINT('',#18379);
#5790=VERTEX_POINT('',#18383);
#5791=VERTEX_POINT('',#18385);
#5792=VERTEX_POINT('',#18389);
#5793=VERTEX_POINT('',#18391);
#5794=VERTEX_POINT('',#18395);
#5795=VERTEX_POINT('',#18397);
#5796=VERTEX_POINT('',#18401);
#5797=VERTEX_POINT('',#18403);
#5798=VERTEX_POINT('',#18408);
#5799=VERTEX_POINT('',#18410);
#5800=VERTEX_POINT('',#18417);
#5801=VERTEX_POINT('',#18419);
#5802=VERTEX_POINT('',#18423);
#5803=VERTEX_POINT('',#18425);
#5804=VERTEX_POINT('',#18429);
#5805=VERTEX_POINT('',#18431);
#5806=VERTEX_POINT('',#18435);
#5807=VERTEX_POINT('',#18437);
#5808=VERTEX_POINT('',#18441);
#5809=VERTEX_POINT('',#18443);
#5810=VERTEX_POINT('',#18447);
#5811=VERTEX_POINT('',#18449);
#5812=VERTEX_POINT('',#18454);
#5813=VERTEX_POINT('',#18456);
#5814=VERTEX_POINT('',#18463);
#5815=VERTEX_POINT('',#18464);
#5816=VERTEX_POINT('',#18466);
#5817=VERTEX_POINT('',#18468);
#5818=VERTEX_POINT('',#18472);
#5819=VERTEX_POINT('',#18474);
#5820=VERTEX_POINT('',#18476);
#5821=VERTEX_POINT('',#18479);
#5822=VERTEX_POINT('',#18481);
#5823=VERTEX_POINT('',#18484);
#5824=VERTEX_POINT('',#18486);
#5825=VERTEX_POINT('',#18488);
#5826=VERTEX_POINT('',#18490);
#5827=VERTEX_POINT('',#18492);
#5828=VERTEX_POINT('',#18495);
#5829=VERTEX_POINT('',#18497);
#5830=VERTEX_POINT('',#18499);
#5831=VERTEX_POINT('',#18501);
#5832=VERTEX_POINT('',#18503);
#5833=VERTEX_POINT('',#18506);
#5834=VERTEX_POINT('',#18510);
#5835=VERTEX_POINT('',#18514);
#5836=VERTEX_POINT('',#18518);
#5837=VERTEX_POINT('',#18522);
#5838=VERTEX_POINT('',#18526);
#5839=VERTEX_POINT('',#18530);
#5840=VERTEX_POINT('',#18534);
#5841=VERTEX_POINT('',#18536);
#5842=VERTEX_POINT('',#18540);
#5843=VERTEX_POINT('',#18542);
#5844=VERTEX_POINT('',#18550);
#5845=VERTEX_POINT('',#18554);
#5846=VERTEX_POINT('',#18562);
#5847=VERTEX_POINT('',#18564);
#5848=VERTEX_POINT('',#18568);
#5849=VERTEX_POINT('',#18570);
#5850=VERTEX_POINT('',#18574);
#5851=VERTEX_POINT('',#18576);
#5852=VERTEX_POINT('',#18580);
#5853=VERTEX_POINT('',#18582);
#5854=VERTEX_POINT('',#18586);
#5855=VERTEX_POINT('',#18588);
#5856=VERTEX_POINT('',#18592);
#5857=VERTEX_POINT('',#18594);
#5858=VERTEX_POINT('',#18599);
#5859=VERTEX_POINT('',#18601);
#5860=VERTEX_POINT('',#18608);
#5861=VERTEX_POINT('',#18610);
#5862=VERTEX_POINT('',#18614);
#5863=VERTEX_POINT('',#18616);
#5864=VERTEX_POINT('',#18620);
#5865=VERTEX_POINT('',#18622);
#5866=VERTEX_POINT('',#18626);
#5867=VERTEX_POINT('',#18628);
#5868=VERTEX_POINT('',#18632);
#5869=VERTEX_POINT('',#18634);
#5870=VERTEX_POINT('',#18638);
#5871=VERTEX_POINT('',#18640);
#5872=VERTEX_POINT('',#18645);
#5873=VERTEX_POINT('',#18647);
#5874=VERTEX_POINT('',#18654);
#5875=VERTEX_POINT('',#18657);
#5876=VERTEX_POINT('',#18661);
#5877=VERTEX_POINT('',#18665);
#5878=VERTEX_POINT('',#18669);
#5879=VERTEX_POINT('',#18672);
#5880=VERTEX_POINT('',#18676);
#5881=VERTEX_POINT('',#18680);
#5882=VERTEX_POINT('',#18685);
#5883=VERTEX_POINT('',#18686);
#5884=VERTEX_POINT('',#18688);
#5885=VERTEX_POINT('',#18690);
#5886=VERTEX_POINT('',#18694);
#5887=VERTEX_POINT('',#18696);
#5888=VERTEX_POINT('',#18700);
#5889=VERTEX_POINT('',#18702);
#5890=VERTEX_POINT('',#18706);
#5891=VERTEX_POINT('',#18708);
#5892=VERTEX_POINT('',#18712);
#5893=VERTEX_POINT('',#18714);
#5894=VERTEX_POINT('',#18725);
#5895=VERTEX_POINT('',#18726);
#5896=VERTEX_POINT('',#18729);
#5897=VERTEX_POINT('',#18731);
#5898=VERTEX_POINT('',#18735);
#5899=VERTEX_POINT('',#18739);
#5900=VERTEX_POINT('',#18741);
#5901=VERTEX_POINT('',#18745);
#5902=VERTEX_POINT('',#18750);
#5903=VERTEX_POINT('',#18754);
#5904=VERTEX_POINT('',#18760);
#5905=VERTEX_POINT('',#18761);
#5906=VERTEX_POINT('',#18764);
#5907=VERTEX_POINT('',#18766);
#5908=VERTEX_POINT('',#18770);
#5909=VERTEX_POINT('',#18774);
#5910=VERTEX_POINT('',#18776);
#5911=VERTEX_POINT('',#18779);
#5912=VERTEX_POINT('',#18783);
#5913=VERTEX_POINT('',#18787);
#5914=VERTEX_POINT('',#18795);
#5915=VERTEX_POINT('',#18796);
#5916=VERTEX_POINT('',#18799);
#5917=VERTEX_POINT('',#18800);
#5918=VERTEX_POINT('',#18803);
#5919=VERTEX_POINT('',#18804);
#5920=VERTEX_POINT('',#18807);
#5921=VERTEX_POINT('',#18808);
#5922=VERTEX_POINT('',#18811);
#5923=VERTEX_POINT('',#18812);
#5924=VERTEX_POINT('',#18815);
#5925=VERTEX_POINT('',#18816);
#5926=VERTEX_POINT('',#18819);
#5927=VERTEX_POINT('',#18820);
#5928=VERTEX_POINT('',#18824);
#5929=VERTEX_POINT('',#18825);
#5930=VERTEX_POINT('',#18848);
#5931=VERTEX_POINT('',#18850);
#5932=VERTEX_POINT('',#18875);
#5933=VERTEX_POINT('',#18877);
#5934=VERTEX_POINT('',#18900);
#5935=VERTEX_POINT('',#18902);
#5936=VERTEX_POINT('',#18925);
#5937=VERTEX_POINT('',#18927);
#5938=VERTEX_POINT('',#18930);
#5939=VERTEX_POINT('',#18932);
#5940=VERTEX_POINT('',#18955);
#5941=VERTEX_POINT('',#18957);
#5942=VERTEX_POINT('',#18980);
#5943=VERTEX_POINT('',#18982);
#5944=VERTEX_POINT('',#19005);
#5945=VERTEX_POINT('',#19007);
#5946=VERTEX_POINT('',#19032);
#5947=VERTEX_POINT('',#19036);
#5948=VERTEX_POINT('',#19061);
#5949=VERTEX_POINT('',#19065);
#5950=VERTEX_POINT('',#19090);
#5951=VERTEX_POINT('',#19092);
#5952=VERTEX_POINT('',#19096);
#5953=VERTEX_POINT('',#19121);
#5954=VERTEX_POINT('',#19125);
#5955=VERTEX_POINT('',#19150);
#5956=VERTEX_POINT('',#19154);
#5957=VERTEX_POINT('',#19179);
#5958=VERTEX_POINT('',#19182);
#5959=VERTEX_POINT('',#19184);
#5960=VERTEX_POINT('',#19216);
#5961=VERTEX_POINT('',#19218);
#5962=VERTEX_POINT('',#19221);
#5963=VERTEX_POINT('',#19225);
#5964=VERTEX_POINT('',#19230);
#5965=VERTEX_POINT('',#19232);
#5966=VERTEX_POINT('',#19235);
#5967=VERTEX_POINT('',#19239);
#5968=VERTEX_POINT('',#19250);
#5969=VERTEX_POINT('',#19251);
#5970=VERTEX_POINT('',#19253);
#5971=VERTEX_POINT('',#19255);
#5972=VERTEX_POINT('',#19259);
#5973=VERTEX_POINT('',#19261);
#5974=VERTEX_POINT('',#19265);
#5975=VERTEX_POINT('',#19267);
#5976=VERTEX_POINT('',#19271);
#5977=VERTEX_POINT('',#19273);
#5978=VERTEX_POINT('',#19277);
#5979=VERTEX_POINT('',#19279);
#5980=VERTEX_POINT('',#19288);
#5981=VERTEX_POINT('',#19291);
#5982=VERTEX_POINT('',#19294);
#5983=VERTEX_POINT('',#19298);
#5984=VERTEX_POINT('',#19302);
#5985=VERTEX_POINT('',#19306);
#5986=VERTEX_POINT('',#19309);
#5987=VERTEX_POINT('',#19317);
#5988=VERTEX_POINT('',#19319);
#5989=VERTEX_POINT('',#19324);
#5990=VERTEX_POINT('',#19325);
#5991=VERTEX_POINT('',#19327);
#5992=VERTEX_POINT('',#19329);
#5993=VERTEX_POINT('',#19333);
#5994=VERTEX_POINT('',#19334);
#5995=VERTEX_POINT('',#19336);
#5996=VERTEX_POINT('',#19338);
#5997=VERTEX_POINT('',#19342);
#5998=VERTEX_POINT('',#19344);
#5999=VERTEX_POINT('',#19346);
#6000=VERTEX_POINT('',#19351);
#6001=VERTEX_POINT('',#19353);
#6002=VERTEX_POINT('',#19355);
#6003=VERTEX_POINT('',#19360);
#6004=VERTEX_POINT('',#19362);
#6005=VERTEX_POINT('',#19366);
#6006=VERTEX_POINT('',#19368);
#6007=VERTEX_POINT('',#19372);
#6008=VERTEX_POINT('',#19374);
#6009=VERTEX_POINT('',#19378);
#6010=VERTEX_POINT('',#19380);
#6011=VERTEX_POINT('',#19384);
#6012=VERTEX_POINT('',#19386);
#6013=VERTEX_POINT('',#19390);
#6014=VERTEX_POINT('',#19392);
#6015=VERTEX_POINT('',#19396);
#6016=VERTEX_POINT('',#19398);
#6017=VERTEX_POINT('',#19402);
#6018=VERTEX_POINT('',#19404);
#6019=VERTEX_POINT('',#19408);
#6020=VERTEX_POINT('',#19410);
#6021=VERTEX_POINT('',#19414);
#6022=VERTEX_POINT('',#19416);
#6023=VERTEX_POINT('',#19420);
#6024=VERTEX_POINT('',#19422);
#6025=VERTEX_POINT('',#19426);
#6026=VERTEX_POINT('',#19428);
#6027=VERTEX_POINT('',#19432);
#6028=VERTEX_POINT('',#19434);
#6029=VERTEX_POINT('',#19438);
#6030=VERTEX_POINT('',#19440);
#6031=VERTEX_POINT('',#19444);
#6032=VERTEX_POINT('',#19446);
#6033=VERTEX_POINT('',#19450);
#6034=VERTEX_POINT('',#19452);
#6035=VERTEX_POINT('',#19456);
#6036=VERTEX_POINT('',#19458);
#6037=VERTEX_POINT('',#19462);
#6038=VERTEX_POINT('',#19464);
#6039=VERTEX_POINT('',#19468);
#6040=VERTEX_POINT('',#19470);
#6041=VERTEX_POINT('',#19474);
#6042=VERTEX_POINT('',#19476);
#6043=VERTEX_POINT('',#19480);
#6044=VERTEX_POINT('',#19482);
#6045=VERTEX_POINT('',#19486);
#6046=VERTEX_POINT('',#19488);
#6047=VERTEX_POINT('',#19492);
#6048=VERTEX_POINT('',#19494);
#6049=VERTEX_POINT('',#19498);
#6050=VERTEX_POINT('',#19500);
#6051=VERTEX_POINT('',#19504);
#6052=VERTEX_POINT('',#19506);
#6053=VERTEX_POINT('',#19510);
#6054=VERTEX_POINT('',#19512);
#6055=VERTEX_POINT('',#19516);
#6056=VERTEX_POINT('',#19518);
#6057=VERTEX_POINT('',#19522);
#6058=VERTEX_POINT('',#19524);
#6059=VERTEX_POINT('',#19528);
#6060=VERTEX_POINT('',#19530);
#6061=VERTEX_POINT('',#19534);
#6062=VERTEX_POINT('',#19536);
#6063=VERTEX_POINT('',#19540);
#6064=VERTEX_POINT('',#19542);
#6065=VERTEX_POINT('',#19546);
#6066=VERTEX_POINT('',#19548);
#6067=VERTEX_POINT('',#19552);
#6068=VERTEX_POINT('',#19554);
#6069=VERTEX_POINT('',#19558);
#6070=VERTEX_POINT('',#19560);
#6071=VERTEX_POINT('',#19564);
#6072=VERTEX_POINT('',#19566);
#6073=VERTEX_POINT('',#19570);
#6074=VERTEX_POINT('',#19572);
#6075=VERTEX_POINT('',#19576);
#6076=VERTEX_POINT('',#19578);
#6077=VERTEX_POINT('',#19582);
#6078=VERTEX_POINT('',#19584);
#6079=VERTEX_POINT('',#19588);
#6080=VERTEX_POINT('',#19590);
#6081=VERTEX_POINT('',#19594);
#6082=VERTEX_POINT('',#19596);
#6083=VERTEX_POINT('',#19600);
#6084=VERTEX_POINT('',#19602);
#6085=VERTEX_POINT('',#19606);
#6086=VERTEX_POINT('',#19608);
#6087=VERTEX_POINT('',#19612);
#6088=VERTEX_POINT('',#19614);
#6089=VERTEX_POINT('',#19618);
#6090=VERTEX_POINT('',#19620);
#6091=VERTEX_POINT('',#19624);
#6092=VERTEX_POINT('',#19626);
#6093=VERTEX_POINT('',#19630);
#6094=VERTEX_POINT('',#19632);
#6095=VERTEX_POINT('',#19636);
#6096=VERTEX_POINT('',#19638);
#6097=VERTEX_POINT('',#19642);
#6098=VERTEX_POINT('',#19644);
#6099=VERTEX_POINT('',#19648);
#6100=VERTEX_POINT('',#19650);
#6101=VERTEX_POINT('',#19654);
#6102=VERTEX_POINT('',#19656);
#6103=VERTEX_POINT('',#19660);
#6104=VERTEX_POINT('',#19662);
#6105=VERTEX_POINT('',#19666);
#6106=VERTEX_POINT('',#19668);
#6107=VERTEX_POINT('',#19672);
#6108=VERTEX_POINT('',#19674);
#6109=VERTEX_POINT('',#19678);
#6110=VERTEX_POINT('',#19680);
#6111=VERTEX_POINT('',#19684);
#6112=VERTEX_POINT('',#19686);
#6113=VERTEX_POINT('',#19690);
#6114=VERTEX_POINT('',#19692);
#6115=VERTEX_POINT('',#19696);
#6116=VERTEX_POINT('',#19698);
#6117=VERTEX_POINT('',#19702);
#6118=VERTEX_POINT('',#19704);
#6119=VERTEX_POINT('',#19708);
#6120=VERTEX_POINT('',#19710);
#6121=VERTEX_POINT('',#19714);
#6122=VERTEX_POINT('',#19716);
#6123=VERTEX_POINT('',#19720);
#6124=VERTEX_POINT('',#19722);
#6125=VERTEX_POINT('',#19726);
#6126=VERTEX_POINT('',#19728);
#6127=VERTEX_POINT('',#19732);
#6128=VERTEX_POINT('',#19734);
#6129=VERTEX_POINT('',#19738);
#6130=VERTEX_POINT('',#19740);
#6131=VERTEX_POINT('',#19744);
#6132=VERTEX_POINT('',#19746);
#6133=VERTEX_POINT('',#19750);
#6134=VERTEX_POINT('',#19752);
#6135=VERTEX_POINT('',#19756);
#6136=VERTEX_POINT('',#19758);
#6137=VERTEX_POINT('',#19762);
#6138=VERTEX_POINT('',#19764);
#6139=VERTEX_POINT('',#19768);
#6140=VERTEX_POINT('',#19770);
#6141=VERTEX_POINT('',#19774);
#6142=VERTEX_POINT('',#19776);
#6143=VERTEX_POINT('',#19780);
#6144=VERTEX_POINT('',#19782);
#6145=VERTEX_POINT('',#19786);
#6146=VERTEX_POINT('',#19788);
#6147=VERTEX_POINT('',#19792);
#6148=VERTEX_POINT('',#19794);
#6149=VERTEX_POINT('',#19798);
#6150=VERTEX_POINT('',#19800);
#6151=VERTEX_POINT('',#19804);
#6152=VERTEX_POINT('',#19806);
#6153=VERTEX_POINT('',#19810);
#6154=VERTEX_POINT('',#19812);
#6155=VERTEX_POINT('',#19816);
#6156=VERTEX_POINT('',#19818);
#6157=VERTEX_POINT('',#19822);
#6158=VERTEX_POINT('',#19824);
#6159=VERTEX_POINT('',#19828);
#6160=VERTEX_POINT('',#19830);
#6161=VERTEX_POINT('',#19834);
#6162=VERTEX_POINT('',#19836);
#6163=VERTEX_POINT('',#19840);
#6164=VERTEX_POINT('',#19842);
#6165=VERTEX_POINT('',#19846);
#6166=VERTEX_POINT('',#19848);
#6167=VERTEX_POINT('',#19852);
#6168=VERTEX_POINT('',#19854);
#6169=VERTEX_POINT('',#19858);
#6170=VERTEX_POINT('',#19860);
#6171=VERTEX_POINT('',#19864);
#6172=VERTEX_POINT('',#19866);
#6173=VERTEX_POINT('',#19870);
#6174=VERTEX_POINT('',#19872);
#6175=VERTEX_POINT('',#19876);
#6176=VERTEX_POINT('',#19878);
#6177=VERTEX_POINT('',#19882);
#6178=VERTEX_POINT('',#19884);
#6179=VERTEX_POINT('',#19888);
#6180=VERTEX_POINT('',#19890);
#6181=VERTEX_POINT('',#19894);
#6182=VERTEX_POINT('',#19896);
#6183=VERTEX_POINT('',#19900);
#6184=VERTEX_POINT('',#19902);
#6185=VERTEX_POINT('',#19906);
#6186=VERTEX_POINT('',#19908);
#6187=VERTEX_POINT('',#19912);
#6188=VERTEX_POINT('',#19914);
#6189=VERTEX_POINT('',#19918);
#6190=VERTEX_POINT('',#19920);
#6191=VERTEX_POINT('',#19924);
#6192=VERTEX_POINT('',#19926);
#6193=VERTEX_POINT('',#19930);
#6194=VERTEX_POINT('',#19932);
#6195=VERTEX_POINT('',#19936);
#6196=VERTEX_POINT('',#19938);
#6197=VERTEX_POINT('',#19942);
#6198=VERTEX_POINT('',#19944);
#6199=VERTEX_POINT('',#19948);
#6200=VERTEX_POINT('',#19950);
#6201=VERTEX_POINT('',#19954);
#6202=VERTEX_POINT('',#19956);
#6203=VERTEX_POINT('',#19960);
#6204=VERTEX_POINT('',#19962);
#6205=VERTEX_POINT('',#19966);
#6206=VERTEX_POINT('',#19968);
#6207=VERTEX_POINT('',#19972);
#6208=VERTEX_POINT('',#19974);
#6209=VERTEX_POINT('',#19978);
#6210=VERTEX_POINT('',#19980);
#6211=VERTEX_POINT('',#19984);
#6212=VERTEX_POINT('',#19986);
#6213=VERTEX_POINT('',#19990);
#6214=VERTEX_POINT('',#19992);
#6215=VERTEX_POINT('',#19996);
#6216=VERTEX_POINT('',#19998);
#6217=VERTEX_POINT('',#20002);
#6218=VERTEX_POINT('',#20004);
#6219=VERTEX_POINT('',#20008);
#6220=VERTEX_POINT('',#20010);
#6221=VERTEX_POINT('',#20014);
#6222=VERTEX_POINT('',#20016);
#6223=VERTEX_POINT('',#20020);
#6224=VERTEX_POINT('',#20022);
#6225=VERTEX_POINT('',#20026);
#6226=VERTEX_POINT('',#20028);
#6227=VERTEX_POINT('',#20032);
#6228=VERTEX_POINT('',#20034);
#6229=VERTEX_POINT('',#20038);
#6230=VERTEX_POINT('',#20040);
#6231=VERTEX_POINT('',#20044);
#6232=VERTEX_POINT('',#20046);
#6233=VERTEX_POINT('',#20050);
#6234=VERTEX_POINT('',#20052);
#6235=VERTEX_POINT('',#20056);
#6236=VERTEX_POINT('',#20058);
#6237=VERTEX_POINT('',#20062);
#6238=VERTEX_POINT('',#20064);
#6239=VERTEX_POINT('',#20068);
#6240=VERTEX_POINT('',#20070);
#6241=VERTEX_POINT('',#20074);
#6242=VERTEX_POINT('',#20076);
#6243=VERTEX_POINT('',#20080);
#6244=VERTEX_POINT('',#20082);
#6245=VERTEX_POINT('',#20086);
#6246=VERTEX_POINT('',#20088);
#6247=VERTEX_POINT('',#20092);
#6248=VERTEX_POINT('',#20094);
#6249=VERTEX_POINT('',#20098);
#6250=VERTEX_POINT('',#20100);
#6251=VERTEX_POINT('',#20104);
#6252=VERTEX_POINT('',#20106);
#6253=VERTEX_POINT('',#20110);
#6254=VERTEX_POINT('',#20112);
#6255=VERTEX_POINT('',#20116);
#6256=VERTEX_POINT('',#20118);
#6257=VERTEX_POINT('',#20122);
#6258=VERTEX_POINT('',#20124);
#6259=VERTEX_POINT('',#20128);
#6260=VERTEX_POINT('',#20130);
#6261=VERTEX_POINT('',#20134);
#6262=VERTEX_POINT('',#20136);
#6263=VERTEX_POINT('',#20140);
#6264=VERTEX_POINT('',#20142);
#6265=VERTEX_POINT('',#20146);
#6266=VERTEX_POINT('',#20148);
#6267=VERTEX_POINT('',#20152);
#6268=VERTEX_POINT('',#20154);
#6269=VERTEX_POINT('',#20158);
#6270=VERTEX_POINT('',#20160);
#6271=VERTEX_POINT('',#20164);
#6272=VERTEX_POINT('',#20166);
#6273=VERTEX_POINT('',#20170);
#6274=VERTEX_POINT('',#20172);
#6275=VERTEX_POINT('',#20176);
#6276=VERTEX_POINT('',#20178);
#6277=VERTEX_POINT('',#20182);
#6278=VERTEX_POINT('',#20184);
#6279=VERTEX_POINT('',#20188);
#6280=VERTEX_POINT('',#20190);
#6281=VERTEX_POINT('',#20194);
#6282=VERTEX_POINT('',#20196);
#6283=VERTEX_POINT('',#20200);
#6284=VERTEX_POINT('',#20202);
#6285=VERTEX_POINT('',#20206);
#6286=VERTEX_POINT('',#20208);
#6287=VERTEX_POINT('',#20212);
#6288=VERTEX_POINT('',#20214);
#6289=VERTEX_POINT('',#20218);
#6290=VERTEX_POINT('',#20220);
#6291=VERTEX_POINT('',#20224);
#6292=VERTEX_POINT('',#20226);
#6293=VERTEX_POINT('',#20230);
#6294=VERTEX_POINT('',#20232);
#6295=VERTEX_POINT('',#20236);
#6296=VERTEX_POINT('',#20238);
#6297=VERTEX_POINT('',#20242);
#6298=VERTEX_POINT('',#20244);
#6299=VERTEX_POINT('',#20248);
#6300=VERTEX_POINT('',#20250);
#6301=VERTEX_POINT('',#20254);
#6302=VERTEX_POINT('',#20256);
#6303=VERTEX_POINT('',#20260);
#6304=VERTEX_POINT('',#20262);
#6305=VERTEX_POINT('',#20266);
#6306=VERTEX_POINT('',#20268);
#6307=VERTEX_POINT('',#20272);
#6308=VERTEX_POINT('',#20274);
#6309=VERTEX_POINT('',#20278);
#6310=VERTEX_POINT('',#20280);
#6311=VERTEX_POINT('',#20284);
#6312=VERTEX_POINT('',#20286);
#6313=VERTEX_POINT('',#20290);
#6314=VERTEX_POINT('',#20292);
#6315=VERTEX_POINT('',#20296);
#6316=VERTEX_POINT('',#20298);
#6317=VERTEX_POINT('',#20302);
#6318=VERTEX_POINT('',#20304);
#6319=VERTEX_POINT('',#20308);
#6320=VERTEX_POINT('',#20310);
#6321=VERTEX_POINT('',#20314);
#6322=VERTEX_POINT('',#20316);
#6323=VERTEX_POINT('',#20325);
#6324=VERTEX_POINT('',#20328);
#6325=VERTEX_POINT('',#20335);
#6326=VERTEX_POINT('',#20337);
#6327=VERTEX_POINT('',#20342);
#6328=VERTEX_POINT('',#20344);
#6329=VERTEX_POINT('',#20351);
#6330=VERTEX_POINT('',#20352);
#6331=VERTEX_POINT('',#20389);
#6332=VERTEX_POINT('',#20391);
#6333=VERTEX_POINT('',#20429);
#6334=VERTEX_POINT('',#20430);
#6335=VERTEX_POINT('',#20432);
#6336=VERTEX_POINT('',#20434);
#6337=VERTEX_POINT('',#20438);
#6338=VERTEX_POINT('',#20439);
#6339=VERTEX_POINT('',#20441);
#6340=VERTEX_POINT('',#20443);
#6341=VERTEX_POINT('',#20447);
#6342=VERTEX_POINT('',#20449);
#6343=VERTEX_POINT('',#20453);
#6344=VERTEX_POINT('',#20455);
#6345=VERTEX_POINT('',#20468);
#6346=VERTEX_POINT('',#20469);
#6347=VERTEX_POINT('',#20471);
#6348=VERTEX_POINT('',#20473);
#6349=VERTEX_POINT('',#20477);
#6350=VERTEX_POINT('',#20479);
#6351=VERTEX_POINT('',#20483);
#6352=VERTEX_POINT('',#20485);
#6353=VERTEX_POINT('',#20489);
#6354=VERTEX_POINT('',#20491);
#6355=VERTEX_POINT('',#20495);
#6356=VERTEX_POINT('',#20497);
#6357=VERTEX_POINT('',#20505);
#6358=VERTEX_POINT('',#20508);
#6359=VERTEX_POINT('',#20512);
#6360=VERTEX_POINT('',#20516);
#6361=VERTEX_POINT('',#20527);
#6362=VERTEX_POINT('',#20529);
#6363=VERTEX_POINT('',#20534);
#6364=VERTEX_POINT('',#20536);
#6365=VERTEX_POINT('',#20541);
#6366=VERTEX_POINT('',#20542);
#6367=VERTEX_POINT('',#20544);
#6368=VERTEX_POINT('',#20546);
#6369=VERTEX_POINT('',#20550);
#6370=VERTEX_POINT('',#20552);
#6371=VERTEX_POINT('',#20556);
#6372=VERTEX_POINT('',#20560);
#6373=VERTEX_POINT('',#20566);
#6374=VERTEX_POINT('',#20567);
#6375=VERTEX_POINT('',#20569);
#6376=VERTEX_POINT('',#20571);
#6377=VERTEX_POINT('',#20575);
#6378=VERTEX_POINT('',#20577);
#6379=VERTEX_POINT('',#20581);
#6380=VERTEX_POINT('',#20585);
#6381=VERTEX_POINT('',#20591);
#6382=VERTEX_POINT('',#20593);
#6383=VERTEX_POINT('',#20600);
#6384=VERTEX_POINT('',#20602);
#6385=VERTEX_POINT('',#20606);
#6386=VERTEX_POINT('',#20608);
#6387=VERTEX_POINT('',#20615);
#6388=VERTEX_POINT('',#20617);
#6389=VERTEX_POINT('',#20621);
#6390=VERTEX_POINT('',#20623);
#6391=VERTEX_POINT('',#20630);
#6392=VERTEX_POINT('',#20632);
#6393=VERTEX_POINT('',#20636);
#6394=VERTEX_POINT('',#20638);
#6395=VERTEX_POINT('',#20645);
#6396=VERTEX_POINT('',#20647);
#6397=VERTEX_POINT('',#20651);
#6398=VERTEX_POINT('',#20653);
#6399=VERTEX_POINT('',#20660);
#6400=VERTEX_POINT('',#20661);
#6401=VERTEX_POINT('',#20663);
#6402=VERTEX_POINT('',#20665);
#6403=VERTEX_POINT('',#20669);
#6404=VERTEX_POINT('',#20671);
#6405=VERTEX_POINT('',#20675);
#6406=VERTEX_POINT('',#20677);
#6407=VERTEX_POINT('',#20687);
#6408=VERTEX_POINT('',#20688);
#6409=VERTEX_POINT('',#20690);
#6410=VERTEX_POINT('',#20692);
#6411=VERTEX_POINT('',#20696);
#6412=VERTEX_POINT('',#20698);
#6413=VERTEX_POINT('',#20702);
#6414=VERTEX_POINT('',#20704);
#6415=VERTEX_POINT('',#20714);
#6416=VERTEX_POINT('',#20716);
#6417=VERTEX_POINT('',#20720);
#6418=VERTEX_POINT('',#20721);
#6419=VERTEX_POINT('',#20723);
#6420=VERTEX_POINT('',#20725);
#6421=VERTEX_POINT('',#20729);
#6422=VERTEX_POINT('',#20731);
#6423=VERTEX_POINT('',#20735);
#6424=VERTEX_POINT('',#20737);
#6425=VERTEX_POINT('',#20741);
#6426=VERTEX_POINT('',#20747);
#6427=VERTEX_POINT('',#20748);
#6428=VERTEX_POINT('',#20750);
#6429=VERTEX_POINT('',#20752);
#6430=VERTEX_POINT('',#20756);
#6431=VERTEX_POINT('',#20758);
#6432=VERTEX_POINT('',#20762);
#6433=VERTEX_POINT('',#20766);
#6434=VERTEX_POINT('',#20772);
#6435=VERTEX_POINT('',#20778);
#6436=VERTEX_POINT('',#20780);
#6437=VERTEX_POINT('',#20784);
#6438=VERTEX_POINT('',#20786);
#6439=VERTEX_POINT('',#20793);
#6440=VERTEX_POINT('',#20795);
#6441=VERTEX_POINT('',#20799);
#6442=VERTEX_POINT('',#20801);
#6443=VERTEX_POINT('',#20808);
#6444=VERTEX_POINT('',#20810);
#6445=VERTEX_POINT('',#20814);
#6446=VERTEX_POINT('',#20816);
#6447=VERTEX_POINT('',#20823);
#6448=VERTEX_POINT('',#20824);
#6449=VERTEX_POINT('',#20826);
#6450=VERTEX_POINT('',#20828);
#6451=VERTEX_POINT('',#20832);
#6452=VERTEX_POINT('',#20834);
#6453=VERTEX_POINT('',#20838);
#6454=VERTEX_POINT('',#20840);
#6455=VERTEX_POINT('',#20844);
#6456=VERTEX_POINT('',#20845);
#6457=VERTEX_POINT('',#20847);
#6458=VERTEX_POINT('',#20918);
#6459=VERTEX_POINT('',#20920);
#6460=VERTEX_POINT('',#20991);
#6461=VERTEX_POINT('',#20993);
#6462=VERTEX_POINT('',#21064);
#6463=VERTEX_POINT('',#21066);
#6464=VERTEX_POINT('',#21137);
#6465=VERTEX_POINT('',#21139);
#6466=VERTEX_POINT('',#21210);
#6467=VERTEX_POINT('',#21212);
#6468=VERTEX_POINT('',#21283);
#6469=VERTEX_POINT('',#21285);
#6470=VERTEX_POINT('',#21356);
#6471=VERTEX_POINT('',#21358);
#6472=VERTEX_POINT('',#21429);
#6473=VERTEX_POINT('',#21431);
#6474=VERTEX_POINT('',#21502);
#6475=VERTEX_POINT('',#21504);
#6476=VERTEX_POINT('',#21575);
#6477=VERTEX_POINT('',#21577);
#6478=VERTEX_POINT('',#21648);
#6479=VERTEX_POINT('',#21650);
#6480=VERTEX_POINT('',#21721);
#6481=VERTEX_POINT('',#21723);
#6482=VERTEX_POINT('',#21794);
#6483=VERTEX_POINT('',#21796);
#6484=VERTEX_POINT('',#21867);
#6485=VERTEX_POINT('',#21869);
#6486=VERTEX_POINT('',#21940);
#6487=VERTEX_POINT('',#21942);
#6488=VERTEX_POINT('',#22013);
#6489=VERTEX_POINT('',#22015);
#6490=VERTEX_POINT('',#22086);
#6491=VERTEX_POINT('',#22088);
#6492=VERTEX_POINT('',#22159);
#6493=VERTEX_POINT('',#22161);
#6494=VERTEX_POINT('',#22232);
#6495=VERTEX_POINT('',#22234);
#6496=VERTEX_POINT('',#22305);
#6497=VERTEX_POINT('',#22307);
#6498=VERTEX_POINT('',#22378);
#6499=VERTEX_POINT('',#22380);
#6500=VERTEX_POINT('',#22451);
#6501=VERTEX_POINT('',#22453);
#6502=VERTEX_POINT('',#22524);
#6503=VERTEX_POINT('',#22526);
#6504=VERTEX_POINT('',#22597);
#6505=VERTEX_POINT('',#22599);
#6506=VERTEX_POINT('',#22670);
#6507=VERTEX_POINT('',#22672);
#6508=VERTEX_POINT('',#22743);
#6509=VERTEX_POINT('',#22745);
#6510=VERTEX_POINT('',#22816);
#6511=VERTEX_POINT('',#22818);
#6512=VERTEX_POINT('',#22889);
#6513=VERTEX_POINT('',#22891);
#6514=VERTEX_POINT('',#22962);
#6515=VERTEX_POINT('',#22964);
#6516=VERTEX_POINT('',#23035);
#6517=VERTEX_POINT('',#23037);
#6518=VERTEX_POINT('',#23108);
#6519=VERTEX_POINT('',#23110);
#6520=VERTEX_POINT('',#23181);
#6521=VERTEX_POINT('',#23183);
#6522=VERTEX_POINT('',#23254);
#6523=VERTEX_POINT('',#23256);
#6524=VERTEX_POINT('',#23327);
#6525=VERTEX_POINT('',#23329);
#6526=VERTEX_POINT('',#23400);
#6527=VERTEX_POINT('',#23402);
#6528=VERTEX_POINT('',#23473);
#6529=VERTEX_POINT('',#23475);
#6530=VERTEX_POINT('',#23546);
#6531=VERTEX_POINT('',#23548);
#6532=VERTEX_POINT('',#23619);
#6533=VERTEX_POINT('',#23621);
#6534=VERTEX_POINT('',#23692);
#6535=VERTEX_POINT('',#23768);
#6536=VERTEX_POINT('',#23770);
#6537=VERTEX_POINT('',#23914);
#6538=VERTEX_POINT('',#23916);
#6539=VERTEX_POINT('',#23989);
#6540=VERTEX_POINT('',#24132);
#6541=VERTEX_POINT('',#24205);
#6542=VERTEX_POINT('',#24348);
#6543=VERTEX_POINT('',#24421);
#6544=VERTEX_POINT('',#24564);
#6545=VERTEX_POINT('',#24637);
#6546=VERTEX_POINT('',#24780);
#6547=VERTEX_POINT('',#24853);
#6548=VERTEX_POINT('',#24996);
#6549=VERTEX_POINT('',#25069);
#6550=VERTEX_POINT('',#25212);
#6551=VERTEX_POINT('',#25285);
#6552=VERTEX_POINT('',#25428);
#6553=VERTEX_POINT('',#25501);
#6554=VERTEX_POINT('',#25644);
#6555=VERTEX_POINT('',#25717);
#6556=VERTEX_POINT('',#25860);
#6557=VERTEX_POINT('',#25933);
#6558=VERTEX_POINT('',#26076);
#6559=VERTEX_POINT('',#26149);
#6560=VERTEX_POINT('',#26292);
#6561=VERTEX_POINT('',#26365);
#6562=VERTEX_POINT('',#26508);
#6563=VERTEX_POINT('',#26581);
#6564=VERTEX_POINT('',#26724);
#6565=VERTEX_POINT('',#26797);
#6566=VERTEX_POINT('',#26940);
#6567=VERTEX_POINT('',#27013);
#6568=VERTEX_POINT('',#27156);
#6569=VERTEX_POINT('',#27229);
#6570=VERTEX_POINT('',#27372);
#6571=VERTEX_POINT('',#27445);
#6572=VERTEX_POINT('',#27588);
#6573=VERTEX_POINT('',#27661);
#6574=VERTEX_POINT('',#27804);
#6575=VERTEX_POINT('',#27877);
#6576=VERTEX_POINT('',#28020);
#6577=VERTEX_POINT('',#28093);
#6578=VERTEX_POINT('',#28236);
#6579=VERTEX_POINT('',#28309);
#6580=VERTEX_POINT('',#28452);
#6581=VERTEX_POINT('',#28525);
#6582=VERTEX_POINT('',#28668);
#6583=VERTEX_POINT('',#28741);
#6584=VERTEX_POINT('',#28884);
#6585=VERTEX_POINT('',#28957);
#6586=VERTEX_POINT('',#29100);
#6587=VERTEX_POINT('',#29173);
#6588=VERTEX_POINT('',#29316);
#6589=VERTEX_POINT('',#29389);
#6590=VERTEX_POINT('',#29532);
#6591=VERTEX_POINT('',#29605);
#6592=VERTEX_POINT('',#29748);
#6593=VERTEX_POINT('',#29821);
#6594=VERTEX_POINT('',#29964);
#6595=VERTEX_POINT('',#30037);
#6596=VERTEX_POINT('',#30180);
#6597=VERTEX_POINT('',#30253);
#6598=VERTEX_POINT('',#30396);
#6599=VERTEX_POINT('',#30469);
#6600=VERTEX_POINT('',#30612);
#6601=VERTEX_POINT('',#30685);
#6602=VERTEX_POINT('',#30828);
#6603=VERTEX_POINT('',#30901);
#6604=VERTEX_POINT('',#31044);
#6605=VERTEX_POINT('',#31117);
#6606=VERTEX_POINT('',#31260);
#6607=VERTEX_POINT('',#31333);
#6608=VERTEX_POINT('',#31476);
#6609=VERTEX_POINT('',#31549);
#6610=VERTEX_POINT('',#31692);
#6611=VERTEX_POINT('',#31765);
#6612=VERTEX_POINT('',#31908);
#6613=VERTEX_POINT('',#31981);
#6614=VERTEX_POINT('',#32124);
#6615=VERTEX_POINT('',#32197);
#6616=VERTEX_POINT('',#32340);
#6617=VERTEX_POINT('',#32417);
#6618=VERTEX_POINT('',#32419);
#6619=VERTEX_POINT('',#32423);
#6620=VERTEX_POINT('',#32425);
#6621=VERTEX_POINT('',#32432);
#6622=VERTEX_POINT('',#32435);
#6623=VERTEX_POINT('',#32439);
#6624=VERTEX_POINT('',#32443);
#6625=VERTEX_POINT('',#32447);
#6626=VERTEX_POINT('',#32450);
#6627=VERTEX_POINT('',#32454);
#6628=VERTEX_POINT('',#32458);
#6629=VERTEX_POINT('',#32463);
#6630=VERTEX_POINT('',#32464);
#6631=VERTEX_POINT('',#32466);
#6632=VERTEX_POINT('',#32468);
#6633=VERTEX_POINT('',#32472);
#6634=VERTEX_POINT('',#32474);
#6635=VERTEX_POINT('',#32478);
#6636=VERTEX_POINT('',#32480);
#6637=VERTEX_POINT('',#32484);
#6638=VERTEX_POINT('',#32486);
#6639=VERTEX_POINT('',#32490);
#6640=VERTEX_POINT('',#32492);
#6641=VERTEX_POINT('',#32502);
#6642=VERTEX_POINT('',#32505);
#6643=VERTEX_POINT('',#32509);
#6644=VERTEX_POINT('',#32513);
#6645=VERTEX_POINT('',#32517);
#6646=VERTEX_POINT('',#32520);
#6647=VERTEX_POINT('',#32524);
#6648=VERTEX_POINT('',#32528);
#6649=VERTEX_POINT('',#32533);
#6650=VERTEX_POINT('',#32534);
#6651=VERTEX_POINT('',#32536);
#6652=VERTEX_POINT('',#32538);
#6653=VERTEX_POINT('',#32542);
#6654=VERTEX_POINT('',#32544);
#6655=VERTEX_POINT('',#32548);
#6656=VERTEX_POINT('',#32550);
#6657=VERTEX_POINT('',#32554);
#6658=VERTEX_POINT('',#32556);
#6659=VERTEX_POINT('',#32560);
#6660=VERTEX_POINT('',#32562);
#6661=VERTEX_POINT('',#32636);
#6662=VERTEX_POINT('',#32638);
#6663=VERTEX_POINT('',#32642);
#6664=VERTEX_POINT('',#32644);
#6665=EDGE_CURVE('',#5556,#5556,#5166,.T.);
#6666=EDGE_CURVE('',#5556,#5557,#2824,.T.);
#6667=EDGE_CURVE('',#5557,#5557,#5167,.T.);
#6668=EDGE_CURVE('',#5558,#5558,#5168,.T.);
#6669=EDGE_CURVE('',#5558,#5559,#2825,.T.);
#6670=EDGE_CURVE('',#5559,#5559,#5169,.T.);
#6671=EDGE_CURVE('',#5560,#5560,#5170,.T.);
#6672=EDGE_CURVE('',#5560,#5561,#2826,.T.);
#6673=EDGE_CURVE('',#5561,#5561,#5171,.T.);
#6674=EDGE_CURVE('',#5562,#5562,#5172,.T.);
#6675=EDGE_CURVE('',#5562,#5563,#2827,.T.);
#6676=EDGE_CURVE('',#5563,#5563,#5173,.T.);
#6677=EDGE_CURVE('',#5564,#5564,#5174,.T.);
#6678=EDGE_CURVE('',#5564,#5565,#2828,.T.);
#6679=EDGE_CURVE('',#5565,#5565,#5175,.T.);
#6680=EDGE_CURVE('',#5566,#5566,#5176,.T.);
#6681=EDGE_CURVE('',#5566,#5567,#2829,.T.);
#6682=EDGE_CURVE('',#5567,#5567,#5177,.T.);
#6683=EDGE_CURVE('',#5568,#5568,#5178,.T.);
#6684=EDGE_CURVE('',#5568,#5569,#2830,.T.);
#6685=EDGE_CURVE('',#5569,#5569,#5179,.T.);
#6686=EDGE_CURVE('',#5570,#5570,#5180,.T.);
#6687=EDGE_CURVE('',#5570,#5571,#2831,.T.);
#6688=EDGE_CURVE('',#5571,#5571,#5181,.T.);
#6689=EDGE_CURVE('',#5572,#5572,#5182,.T.);
#6690=EDGE_CURVE('',#5572,#5573,#2832,.T.);
#6691=EDGE_CURVE('',#5573,#5573,#5183,.T.);
#6692=EDGE_CURVE('',#5574,#5574,#5184,.T.);
#6693=EDGE_CURVE('',#5574,#5575,#2833,.T.);
#6694=EDGE_CURVE('',#5575,#5575,#5185,.T.);
#6695=EDGE_CURVE('',#5576,#5577,#2834,.T.);
#6696=EDGE_CURVE('',#5577,#5578,#2835,.T.);
#6697=EDGE_CURVE('',#5579,#5578,#2836,.T.);
#6698=EDGE_CURVE('',#5576,#5579,#2837,.T.);
#6699=EDGE_CURVE('',#5580,#5576,#2838,.T.);
#6700=EDGE_CURVE('',#5581,#5579,#2839,.T.);
#6701=EDGE_CURVE('',#5580,#5581,#2840,.T.);
#6702=EDGE_CURVE('',#5582,#5580,#2841,.T.);
#6703=EDGE_CURVE('',#5583,#5581,#2842,.T.);
#6704=EDGE_CURVE('',#5582,#5583,#2843,.T.);
#6705=EDGE_CURVE('',#5577,#5582,#2844,.T.);
#6706=EDGE_CURVE('',#5578,#5583,#2845,.T.);
#6707=EDGE_CURVE('',#5584,#5585,#2846,.T.);
#6708=EDGE_CURVE('',#5585,#5586,#2847,.T.);
#6709=EDGE_CURVE('',#5587,#5586,#2848,.T.);
#6710=EDGE_CURVE('',#5584,#5587,#2849,.T.);
#6711=EDGE_CURVE('',#5588,#5584,#2850,.T.);
#6712=EDGE_CURVE('',#5589,#5587,#2851,.T.);
#6713=EDGE_CURVE('',#5588,#5589,#2852,.T.);
#6714=EDGE_CURVE('',#5590,#5588,#2853,.T.);
#6715=EDGE_CURVE('',#5591,#5589,#2854,.T.);
#6716=EDGE_CURVE('',#5590,#5591,#2855,.T.);
#6717=EDGE_CURVE('',#5585,#5590,#2856,.T.);
#6718=EDGE_CURVE('',#5586,#5591,#2857,.T.);
#6719=EDGE_CURVE('',#5592,#5593,#2858,.T.);
#6720=EDGE_CURVE('',#5593,#5594,#2859,.T.);
#6721=EDGE_CURVE('',#5595,#5594,#2860,.T.);
#6722=EDGE_CURVE('',#5592,#5595,#2861,.T.);
#6723=EDGE_CURVE('',#5596,#5592,#2862,.T.);
#6724=EDGE_CURVE('',#5597,#5595,#2863,.T.);
#6725=EDGE_CURVE('',#5596,#5597,#2864,.T.);
#6726=EDGE_CURVE('',#5598,#5596,#2865,.T.);
#6727=EDGE_CURVE('',#5599,#5597,#2866,.T.);
#6728=EDGE_CURVE('',#5598,#5599,#2867,.T.);
#6729=EDGE_CURVE('',#5593,#5598,#2868,.T.);
#6730=EDGE_CURVE('',#5594,#5599,#2869,.T.);
#6731=EDGE_CURVE('',#5600,#5600,#5186,.T.);
#6732=EDGE_CURVE('',#5600,#5601,#2870,.T.);
#6733=EDGE_CURVE('',#5601,#5601,#5187,.T.);
#6734=EDGE_CURVE('',#5602,#5602,#5188,.T.);
#6735=EDGE_CURVE('',#5602,#5603,#2871,.T.);
#6736=EDGE_CURVE('',#5603,#5603,#5189,.T.);
#6737=EDGE_CURVE('',#5604,#5605,#2872,.T.);
#6738=EDGE_CURVE('',#5606,#5604,#2873,.T.);
#6739=EDGE_CURVE('',#5607,#5606,#2874,.T.);
#6740=EDGE_CURVE('',#5605,#5607,#2875,.T.);
#6741=EDGE_CURVE('',#5608,#5609,#2876,.T.);
#6742=EDGE_CURVE('',#5610,#5608,#2877,.T.);
#6743=EDGE_CURVE('',#5611,#5610,#2878,.T.);
#6744=EDGE_CURVE('',#5609,#5611,#2879,.T.);
#6745=EDGE_CURVE('',#5612,#5604,#5190,.T.);
#6746=EDGE_CURVE('',#5613,#5612,#2880,.T.);
#6747=EDGE_CURVE('',#5614,#5613,#2881,.T.);
#6748=EDGE_CURVE('',#5615,#5614,#2882,.T.);
#6749=EDGE_CURVE('',#5609,#5615,#5191,.T.);
#6750=EDGE_CURVE('',#5611,#5606,#5192,.T.);
#6751=EDGE_CURVE('',#5607,#5610,#5193,.T.);
#6752=EDGE_CURVE('',#5615,#5616,#2883,.T.);
#6753=EDGE_CURVE('',#5608,#5616,#5194,.T.);
#6754=EDGE_CURVE('',#5617,#5605,#5195,.T.);
#6755=EDGE_CURVE('',#5612,#5617,#2884,.T.);
#6756=EDGE_CURVE('',#5616,#5618,#2885,.T.);
#6757=EDGE_CURVE('',#5619,#5618,#2886,.T.);
#6758=EDGE_CURVE('',#5619,#5617,#2887,.T.);
#6759=EDGE_CURVE('',#5618,#5614,#2888,.T.);
#6760=EDGE_CURVE('',#5613,#5619,#2889,.T.);
#6761=EDGE_CURVE('',#5620,#5620,#5196,.T.);
#6762=EDGE_CURVE('',#5620,#5621,#2890,.T.);
#6763=EDGE_CURVE('',#5621,#5621,#5197,.T.);
#6764=EDGE_CURVE('',#5622,#5622,#5198,.T.);
#6765=EDGE_CURVE('',#5622,#5623,#2891,.T.);
#6766=EDGE_CURVE('',#5623,#5623,#5199,.T.);
#6767=EDGE_CURVE('',#5624,#5625,#2892,.T.);
#6768=EDGE_CURVE('',#5626,#5624,#2893,.T.);
#6769=EDGE_CURVE('',#5627,#5626,#2894,.T.);
#6770=EDGE_CURVE('',#5625,#5627,#2895,.T.);
#6771=EDGE_CURVE('',#5628,#5629,#2896,.T.);
#6772=EDGE_CURVE('',#5630,#5628,#2897,.T.);
#6773=EDGE_CURVE('',#5631,#5630,#2898,.T.);
#6774=EDGE_CURVE('',#5629,#5631,#2899,.T.);
#6775=EDGE_CURVE('',#5632,#5624,#5200,.T.);
#6776=EDGE_CURVE('',#5633,#5632,#2900,.T.);
#6777=EDGE_CURVE('',#5634,#5633,#2901,.T.);
#6778=EDGE_CURVE('',#5635,#5634,#2902,.T.);
#6779=EDGE_CURVE('',#5629,#5635,#5201,.T.);
#6780=EDGE_CURVE('',#5631,#5626,#5202,.T.);
#6781=EDGE_CURVE('',#5627,#5630,#5203,.T.);
#6782=EDGE_CURVE('',#5635,#5636,#2903,.T.);
#6783=EDGE_CURVE('',#5628,#5636,#5204,.T.);
#6784=EDGE_CURVE('',#5637,#5625,#5205,.T.);
#6785=EDGE_CURVE('',#5632,#5637,#2904,.T.);
#6786=EDGE_CURVE('',#5636,#5638,#2905,.T.);
#6787=EDGE_CURVE('',#5639,#5638,#2906,.T.);
#6788=EDGE_CURVE('',#5639,#5637,#2907,.T.);
#6789=EDGE_CURVE('',#5638,#5634,#2908,.T.);
#6790=EDGE_CURVE('',#5633,#5639,#2909,.T.);
#6791=EDGE_CURVE('',#5640,#5640,#5206,.T.);
#6792=EDGE_CURVE('',#5640,#5641,#2910,.T.);
#6793=EDGE_CURVE('',#5641,#5641,#5207,.T.);
#6794=EDGE_CURVE('',#5642,#5642,#5208,.T.);
#6795=EDGE_CURVE('',#5642,#5643,#2911,.T.);
#6796=EDGE_CURVE('',#5643,#5643,#5209,.T.);
#6797=EDGE_CURVE('',#5644,#5644,#5210,.T.);
#6798=EDGE_CURVE('',#5644,#5645,#2912,.T.);
#6799=EDGE_CURVE('',#5645,#5645,#5211,.T.);
#6800=EDGE_CURVE('',#5646,#5646,#5212,.T.);
#6801=EDGE_CURVE('',#5646,#5647,#2913,.T.);
#6802=EDGE_CURVE('',#5647,#5647,#5213,.T.);
#6803=EDGE_CURVE('',#5648,#5649,#2914,.T.);
#6804=EDGE_CURVE('',#5649,#5650,#2915,.T.);
#6805=EDGE_CURVE('',#5650,#5651,#2916,.T.);
#6806=EDGE_CURVE('',#5651,#5648,#2917,.T.);
#6807=EDGE_CURVE('',#5652,#5653,#2918,.T.);
#6808=EDGE_CURVE('',#5654,#5652,#2919,.T.);
#6809=EDGE_CURVE('',#5655,#5654,#2920,.T.);
#6810=EDGE_CURVE('',#5653,#5655,#2921,.T.);
#6811=EDGE_CURVE('',#5656,#5657,#2922,.T.);
#6812=EDGE_CURVE('',#5657,#5648,#2923,.T.);
#6813=EDGE_CURVE('',#5656,#5651,#2924,.T.);
#6814=EDGE_CURVE('',#5658,#5656,#2925,.T.);
#6815=EDGE_CURVE('',#5658,#5650,#2926,.T.);
#6816=EDGE_CURVE('',#5659,#5658,#2927,.T.);
#6817=EDGE_CURVE('',#5659,#5649,#2928,.T.);
#6818=EDGE_CURVE('',#5657,#5659,#2929,.T.);
#6819=EDGE_CURVE('',#5654,#5660,#2930,.T.);
#6820=EDGE_CURVE('',#5661,#5660,#2931,.T.);
#6821=EDGE_CURVE('',#5655,#5661,#2932,.T.);
#6822=EDGE_CURVE('',#5652,#5662,#2933,.T.);
#6823=EDGE_CURVE('',#5660,#5662,#2934,.T.);
#6824=EDGE_CURVE('',#5653,#5663,#2935,.T.);
#6825=EDGE_CURVE('',#5662,#5663,#2936,.T.);
#6826=EDGE_CURVE('',#5663,#5661,#2937,.T.);
#6827=EDGE_CURVE('',#5664,#5665,#2938,.T.);
#6828=EDGE_CURVE('',#5664,#5666,#2939,.T.);
#6829=EDGE_CURVE('',#5667,#5666,#2940,.T.);
#6830=EDGE_CURVE('',#5665,#5667,#2941,.T.);
#6831=EDGE_CURVE('',#5668,#5669,#2942,.T.);
#6832=EDGE_CURVE('',#5670,#5668,#2943,.T.);
#6833=EDGE_CURVE('',#5671,#5670,#2944,.T.);
#6834=EDGE_CURVE('',#5669,#5671,#2945,.T.);
#6835=EDGE_CURVE('',#5672,#5668,#2946,.T.);
#6836=EDGE_CURVE('',#5673,#5672,#2947,.T.);
#6837=EDGE_CURVE('',#5674,#5673,#2948,.T.);
#6838=EDGE_CURVE('',#5675,#5674,#2949,.T.);
#6839=EDGE_CURVE('',#5670,#5675,#2950,.T.);
#6840=EDGE_CURVE('',#5676,#5664,#2951,.T.);
#6841=EDGE_CURVE('',#5677,#5676,#2952,.T.);
#6842=EDGE_CURVE('',#5678,#5677,#2953,.T.);
#6843=EDGE_CURVE('',#5679,#5678,#2954,.T.);
#6844=EDGE_CURVE('',#5666,#5679,#2955,.T.);
#6845=EDGE_CURVE('',#5676,#5675,#5214,.T.);
#6846=EDGE_CURVE('',#5671,#5665,#5215,.T.);
#6847=EDGE_CURVE('',#5669,#5667,#5216,.T.);
#6848=EDGE_CURVE('',#5677,#5674,#5217,.T.);
#6849=EDGE_CURVE('',#5678,#5673,#5218,.T.);
#6850=EDGE_CURVE('',#5679,#5672,#5219,.T.);
#6851=EDGE_CURVE('',#5680,#5680,#5220,.T.);
#6852=EDGE_CURVE('',#5680,#5681,#2956,.T.);
#6853=EDGE_CURVE('',#5681,#5681,#5221,.T.);
#6854=EDGE_CURVE('',#5682,#5682,#5222,.T.);
#6855=EDGE_CURVE('',#5682,#5683,#2957,.T.);
#6856=EDGE_CURVE('',#5683,#5683,#5223,.T.);
#6857=EDGE_CURVE('',#5684,#5685,#2958,.T.);
#6858=EDGE_CURVE('',#5684,#5686,#2959,.T.);
#6859=EDGE_CURVE('',#5687,#5686,#2960,.T.);
#6860=EDGE_CURVE('',#5685,#5687,#2961,.T.);
#6861=EDGE_CURVE('',#5688,#5689,#2962,.T.);
#6862=EDGE_CURVE('',#5690,#5688,#2963,.T.);
#6863=EDGE_CURVE('',#5691,#5690,#2964,.T.);
#6864=EDGE_CURVE('',#5689,#5691,#2965,.T.);
#6865=EDGE_CURVE('',#5692,#5688,#2966,.T.);
#6866=EDGE_CURVE('',#5693,#5692,#2967,.T.);
#6867=EDGE_CURVE('',#5690,#5693,#2968,.T.);
#6868=EDGE_CURVE('',#5694,#5684,#2969,.T.);
#6869=EDGE_CURVE('',#5695,#5694,#2970,.T.);
#6870=EDGE_CURVE('',#5686,#5695,#2971,.T.);
#6871=EDGE_CURVE('',#5696,#5687,#2972,.T.);
#6872=EDGE_CURVE('',#5697,#5696,#2973,.T.);
#6873=EDGE_CURVE('',#5697,#5685,#2974,.T.);
#6874=EDGE_CURVE('',#5691,#5698,#2975,.T.);
#6875=EDGE_CURVE('',#5698,#5699,#2976,.T.);
#6876=EDGE_CURVE('',#5689,#5699,#2977,.T.);
#6877=EDGE_CURVE('',#5695,#5692,#5224,.T.);
#6878=EDGE_CURVE('',#5699,#5700,#2978,.T.);
#6879=EDGE_CURVE('',#5700,#5701,#2979,.T.);
#6880=EDGE_CURVE('',#5701,#5696,#2980,.T.);
#6881=EDGE_CURVE('',#5693,#5694,#5225,.T.);
#6882=EDGE_CURVE('',#5702,#5697,#2981,.T.);
#6883=EDGE_CURVE('',#5702,#5701,#2982,.T.);
#6884=EDGE_CURVE('',#5703,#5702,#2983,.T.);
#6885=EDGE_CURVE('',#5703,#5700,#2984,.T.);
#6886=EDGE_CURVE('',#5698,#5703,#2985,.T.);
#6887=EDGE_CURVE('',#5704,#5705,#2986,.T.);
#6888=EDGE_CURVE('',#5704,#5706,#2987,.T.);
#6889=EDGE_CURVE('',#5707,#5706,#2988,.T.);
#6890=EDGE_CURVE('',#5705,#5707,#2989,.T.);
#6891=EDGE_CURVE('',#5708,#5709,#2990,.T.);
#6892=EDGE_CURVE('',#5710,#5708,#2991,.T.);
#6893=EDGE_CURVE('',#5711,#5710,#2992,.T.);
#6894=EDGE_CURVE('',#5709,#5711,#2993,.T.);
#6895=EDGE_CURVE('',#5712,#5708,#2994,.T.);
#6896=EDGE_CURVE('',#5713,#5712,#2995,.T.);
#6897=EDGE_CURVE('',#5714,#5713,#2996,.T.);
#6898=EDGE_CURVE('',#5715,#5714,#2997,.T.);
#6899=EDGE_CURVE('',#5710,#5715,#2998,.T.);
#6900=EDGE_CURVE('',#5716,#5704,#2999,.T.);
#6901=EDGE_CURVE('',#5717,#5716,#3000,.T.);
#6902=EDGE_CURVE('',#5718,#5717,#3001,.T.);
#6903=EDGE_CURVE('',#5719,#5718,#3002,.T.);
#6904=EDGE_CURVE('',#5706,#5719,#3003,.T.);
#6905=EDGE_CURVE('',#5716,#5715,#5226,.T.);
#6906=EDGE_CURVE('',#5711,#5705,#5227,.T.);
#6907=EDGE_CURVE('',#5709,#5707,#5228,.T.);
#6908=EDGE_CURVE('',#5717,#5714,#5229,.T.);
#6909=EDGE_CURVE('',#5718,#5713,#5230,.T.);
#6910=EDGE_CURVE('',#5719,#5712,#5231,.T.);
#6911=EDGE_CURVE('',#5720,#5720,#5232,.T.);
#6912=EDGE_CURVE('',#5720,#5721,#3004,.T.);
#6913=EDGE_CURVE('',#5721,#5721,#5233,.T.);
#6914=EDGE_CURVE('',#5722,#5722,#5234,.T.);
#6915=EDGE_CURVE('',#5722,#5723,#3005,.T.);
#6916=EDGE_CURVE('',#5723,#5723,#5235,.T.);
#6917=EDGE_CURVE('',#5724,#5725,#3006,.T.);
#6918=EDGE_CURVE('',#5724,#5726,#3007,.T.);
#6919=EDGE_CURVE('',#5727,#5726,#3008,.T.);
#6920=EDGE_CURVE('',#5725,#5727,#3009,.T.);
#6921=EDGE_CURVE('',#5728,#5729,#3010,.T.);
#6922=EDGE_CURVE('',#5730,#5728,#3011,.T.);
#6923=EDGE_CURVE('',#5731,#5730,#3012,.T.);
#6924=EDGE_CURVE('',#5729,#5731,#3013,.T.);
#6925=EDGE_CURVE('',#5732,#5728,#3014,.T.);
#6926=EDGE_CURVE('',#5733,#5732,#3015,.T.);
#6927=EDGE_CURVE('',#5730,#5733,#3016,.T.);
#6928=EDGE_CURVE('',#5734,#5724,#3017,.T.);
#6929=EDGE_CURVE('',#5735,#5734,#3018,.T.);
#6930=EDGE_CURVE('',#5726,#5735,#3019,.T.);
#6931=EDGE_CURVE('',#5736,#5727,#3020,.T.);
#6932=EDGE_CURVE('',#5737,#5736,#3021,.T.);
#6933=EDGE_CURVE('',#5737,#5725,#3022,.T.);
#6934=EDGE_CURVE('',#5731,#5738,#3023,.T.);
#6935=EDGE_CURVE('',#5738,#5739,#3024,.T.);
#6936=EDGE_CURVE('',#5729,#5739,#3025,.T.);
#6937=EDGE_CURVE('',#5735,#5732,#5236,.T.);
#6938=EDGE_CURVE('',#5739,#5740,#3026,.T.);
#6939=EDGE_CURVE('',#5740,#5741,#3027,.T.);
#6940=EDGE_CURVE('',#5741,#5736,#3028,.T.);
#6941=EDGE_CURVE('',#5733,#5734,#5237,.T.);
#6942=EDGE_CURVE('',#5742,#5737,#3029,.T.);
#6943=EDGE_CURVE('',#5742,#5741,#3030,.T.);
#6944=EDGE_CURVE('',#5743,#5742,#3031,.T.);
#6945=EDGE_CURVE('',#5743,#5740,#3032,.T.);
#6946=EDGE_CURVE('',#5738,#5743,#3033,.T.);
#6947=EDGE_CURVE('',#5744,#5744,#5238,.T.);
#6948=EDGE_CURVE('',#5744,#5745,#3034,.T.);
#6949=EDGE_CURVE('',#5745,#5745,#5239,.T.);
#6950=EDGE_CURVE('',#5746,#5746,#5240,.T.);
#6951=EDGE_CURVE('',#5747,#5747,#5241,.T.);
#6952=EDGE_CURVE('',#5747,#5748,#3035,.T.);
#6953=EDGE_CURVE('',#5748,#5748,#5242,.T.);
#6954=EDGE_CURVE('',#5749,#5749,#5243,.T.);
#6955=EDGE_CURVE('',#5750,#5750,#5244,.T.);
#6956=EDGE_CURVE('',#5750,#5746,#3036,.T.);
#6957=EDGE_CURVE('',#5751,#5751,#5245,.T.);
#6958=EDGE_CURVE('',#5751,#5749,#3037,.T.);
#6959=EDGE_CURVE('',#5752,#5752,#5246,.T.);
#6960=EDGE_CURVE('',#5752,#5753,#3038,.T.);
#6961=EDGE_CURVE('',#5753,#5753,#5247,.T.);
#6962=EDGE_CURVE('',#5754,#5755,#5248,.T.);
#6963=EDGE_CURVE('',#5756,#5754,#3039,.T.);
#6964=EDGE_CURVE('',#5757,#5756,#5249,.T.);
#6965=EDGE_CURVE('',#5755,#5757,#3040,.T.);
#6966=EDGE_CURVE('',#5758,#5756,#3041,.T.);
#6967=EDGE_CURVE('',#5759,#5758,#3042,.T.);
#6968=EDGE_CURVE('',#5759,#5760,#3043,.T.);
#6969=EDGE_CURVE('',#5757,#5760,#3044,.T.);
#6970=EDGE_CURVE('',#5761,#5761,#5250,.T.);
#6971=EDGE_CURVE('',#5762,#5762,#5251,.T.);
#6972=EDGE_CURVE('',#5763,#5754,#3045,.T.);
#6973=EDGE_CURVE('',#5758,#5763,#3046,.T.);
#6974=EDGE_CURVE('',#5764,#5764,#5252,.T.);
#6975=EDGE_CURVE('',#5764,#5765,#3047,.T.);
#6976=EDGE_CURVE('',#5765,#5765,#5253,.T.);
#6977=EDGE_CURVE('',#5766,#5766,#5254,.T.);
#6978=EDGE_CURVE('',#5766,#5767,#3048,.T.);
#6979=EDGE_CURVE('',#5767,#5767,#5255,.T.);
#6980=EDGE_CURVE('',#5768,#5768,#5256,.T.);
#6981=EDGE_CURVE('',#5768,#5769,#3049,.T.);
#6982=EDGE_CURVE('',#5769,#5769,#5257,.T.);
#6983=EDGE_CURVE('',#5770,#5770,#5258,.T.);
#6984=EDGE_CURVE('',#5770,#5771,#3050,.T.);
#6985=EDGE_CURVE('',#5771,#5771,#5259,.T.);
#6986=EDGE_CURVE('',#5762,#5772,#3051,.T.);
#6987=EDGE_CURVE('',#5772,#5772,#5260,.T.);
#6988=EDGE_CURVE('',#5761,#5773,#3052,.T.);
#6989=EDGE_CURVE('',#5773,#5773,#5261,.T.);
#6990=EDGE_CURVE('',#5774,#5774,#5262,.T.);
#6991=EDGE_CURVE('',#5774,#5775,#3053,.T.);
#6992=EDGE_CURVE('',#5775,#5775,#5263,.T.);
#6993=EDGE_CURVE('',#5776,#5755,#3054,.T.);
#6994=EDGE_CURVE('',#5777,#5776,#3055,.T.);
#6995=EDGE_CURVE('',#5763,#5777,#3056,.T.);
#6996=EDGE_CURVE('',#5778,#5779,#3057,.T.);
#6997=EDGE_CURVE('',#5780,#5778,#3058,.T.);
#6998=EDGE_CURVE('',#5781,#5780,#3059,.T.);
#6999=EDGE_CURVE('',#5779,#5781,#3060,.T.);
#7000=EDGE_CURVE('',#5781,#5759,#3061,.T.);
#7001=EDGE_CURVE('',#5760,#5780,#3062,.T.);
#7002=EDGE_CURVE('',#5777,#5782,#3063,.T.);
#7003=EDGE_CURVE('',#5783,#5782,#3064,.T.);
#7004=EDGE_CURVE('',#5779,#5783,#3065,.T.);
#7005=EDGE_CURVE('',#5776,#5784,#3066,.T.);
#7006=EDGE_CURVE('',#5782,#5784,#3067,.T.);
#7007=EDGE_CURVE('',#5778,#5785,#3068,.T.);
#7008=EDGE_CURVE('',#5784,#5785,#3069,.T.);
#7009=EDGE_CURVE('',#5785,#5783,#3070,.T.);
#7010=EDGE_CURVE('',#5786,#5786,#5264,.T.);
#7011=EDGE_CURVE('',#5786,#5787,#3071,.T.);
#7012=EDGE_CURVE('',#5787,#5787,#5265,.T.);
#7013=EDGE_CURVE('',#5788,#5788,#5266,.T.);
#7014=EDGE_CURVE('',#5788,#5789,#3072,.T.);
#7015=EDGE_CURVE('',#5789,#5789,#5267,.T.);
#7016=EDGE_CURVE('',#5790,#5790,#5268,.T.);
#7017=EDGE_CURVE('',#5790,#5791,#3073,.T.);
#7018=EDGE_CURVE('',#5791,#5791,#5269,.T.);
#7019=EDGE_CURVE('',#5792,#5792,#5270,.T.);
#7020=EDGE_CURVE('',#5792,#5793,#3074,.T.);
#7021=EDGE_CURVE('',#5793,#5793,#5271,.T.);
#7022=EDGE_CURVE('',#5794,#5794,#5272,.T.);
#7023=EDGE_CURVE('',#5794,#5795,#3075,.T.);
#7024=EDGE_CURVE('',#5795,#5795,#5273,.T.);
#7025=EDGE_CURVE('',#5796,#5796,#5274,.T.);
#7026=EDGE_CURVE('',#5796,#5797,#3076,.T.);
#7027=EDGE_CURVE('',#5797,#5797,#5275,.T.);
#7028=EDGE_CURVE('',#5798,#5798,#5276,.T.);
#7029=EDGE_CURVE('',#5798,#5799,#3077,.T.);
#7030=EDGE_CURVE('',#5799,#5799,#5277,.T.);
#7031=EDGE_CURVE('',#5800,#5800,#5278,.T.);
#7032=EDGE_CURVE('',#5800,#5801,#3078,.T.);
#7033=EDGE_CURVE('',#5801,#5801,#5279,.T.);
#7034=EDGE_CURVE('',#5802,#5802,#5280,.T.);
#7035=EDGE_CURVE('',#5802,#5803,#3079,.T.);
#7036=EDGE_CURVE('',#5803,#5803,#5281,.T.);
#7037=EDGE_CURVE('',#5804,#5804,#5282,.T.);
#7038=EDGE_CURVE('',#5804,#5805,#3080,.T.);
#7039=EDGE_CURVE('',#5805,#5805,#5283,.T.);
#7040=EDGE_CURVE('',#5806,#5806,#5284,.T.);
#7041=EDGE_CURVE('',#5806,#5807,#3081,.T.);
#7042=EDGE_CURVE('',#5807,#5807,#5285,.T.);
#7043=EDGE_CURVE('',#5808,#5808,#5286,.T.);
#7044=EDGE_CURVE('',#5808,#5809,#3082,.T.);
#7045=EDGE_CURVE('',#5809,#5809,#5287,.T.);
#7046=EDGE_CURVE('',#5810,#5810,#5288,.T.);
#7047=EDGE_CURVE('',#5810,#5811,#3083,.T.);
#7048=EDGE_CURVE('',#5811,#5811,#5289,.T.);
#7049=EDGE_CURVE('',#5812,#5812,#5290,.T.);
#7050=EDGE_CURVE('',#5812,#5813,#3084,.T.);
#7051=EDGE_CURVE('',#5813,#5813,#5291,.T.);
#7052=EDGE_CURVE('',#5814,#5815,#5292,.T.);
#7053=EDGE_CURVE('',#5816,#5814,#3085,.T.);
#7054=EDGE_CURVE('',#5817,#5816,#5293,.T.);
#7055=EDGE_CURVE('',#5815,#5817,#3086,.T.);
#7056=EDGE_CURVE('',#5818,#5816,#3087,.T.);
#7057=EDGE_CURVE('',#5818,#5819,#3088,.T.);
#7058=EDGE_CURVE('',#5820,#5819,#3089,.T.);
#7059=EDGE_CURVE('',#5817,#5820,#3090,.T.);
#7060=EDGE_CURVE('',#5821,#5821,#5294,.T.);
#7061=EDGE_CURVE('',#5822,#5822,#5295,.T.);
#7062=EDGE_CURVE('',#5814,#5823,#3091,.T.);
#7063=EDGE_CURVE('',#5823,#5824,#3092,.T.);
#7064=EDGE_CURVE('',#5825,#5824,#3093,.T.);
#7065=EDGE_CURVE('',#5826,#5825,#3094,.T.);
#7066=EDGE_CURVE('',#5826,#5827,#3095,.T.);
#7067=EDGE_CURVE('',#5827,#5818,#3096,.T.);
#7068=EDGE_CURVE('',#5828,#5828,#5296,.T.);
#7069=EDGE_CURVE('',#5829,#5829,#5297,.T.);
#7070=EDGE_CURVE('',#5830,#5830,#5298,.T.);
#7071=EDGE_CURVE('',#5831,#5831,#5299,.T.);
#7072=EDGE_CURVE('',#5832,#5832,#5300,.T.);
#7073=EDGE_CURVE('',#5828,#5833,#3097,.T.);
#7074=EDGE_CURVE('',#5833,#5833,#5301,.T.);
#7075=EDGE_CURVE('',#5829,#5834,#3098,.T.);
#7076=EDGE_CURVE('',#5834,#5834,#5302,.T.);
#7077=EDGE_CURVE('',#5830,#5835,#3099,.T.);
#7078=EDGE_CURVE('',#5835,#5835,#5303,.T.);
#7079=EDGE_CURVE('',#5831,#5836,#3100,.T.);
#7080=EDGE_CURVE('',#5836,#5836,#5304,.T.);
#7081=EDGE_CURVE('',#5822,#5837,#3101,.T.);
#7082=EDGE_CURVE('',#5837,#5837,#5305,.T.);
#7083=EDGE_CURVE('',#5821,#5838,#3102,.T.);
#7084=EDGE_CURVE('',#5838,#5838,#5306,.T.);
#7085=EDGE_CURVE('',#5832,#5839,#3103,.T.);
#7086=EDGE_CURVE('',#5839,#5839,#5307,.T.);
#7087=EDGE_CURVE('',#5815,#5840,#3104,.T.);
#7088=EDGE_CURVE('',#5841,#5840,#3105,.T.);
#7089=EDGE_CURVE('',#5823,#5841,#3106,.T.);
#7090=EDGE_CURVE('',#5842,#5826,#3107,.T.);
#7091=EDGE_CURVE('',#5843,#5842,#3108,.T.);
#7092=EDGE_CURVE('',#5827,#5843,#3109,.T.);
#7093=EDGE_CURVE('',#5819,#5843,#3110,.T.);
#7094=EDGE_CURVE('',#5840,#5820,#3111,.T.);
#7095=EDGE_CURVE('',#5841,#5844,#3112,.T.);
#7096=EDGE_CURVE('',#5824,#5844,#3113,.T.);
#7097=EDGE_CURVE('',#5842,#5845,#3114,.T.);
#7098=EDGE_CURVE('',#5844,#5845,#3115,.T.);
#7099=EDGE_CURVE('',#5845,#5825,#3116,.T.);
#7100=EDGE_CURVE('',#5846,#5846,#5308,.T.);
#7101=EDGE_CURVE('',#5846,#5847,#3117,.T.);
#7102=EDGE_CURVE('',#5847,#5847,#5309,.T.);
#7103=EDGE_CURVE('',#5848,#5848,#5310,.T.);
#7104=EDGE_CURVE('',#5848,#5849,#3118,.T.);
#7105=EDGE_CURVE('',#5849,#5849,#5311,.T.);
#7106=EDGE_CURVE('',#5850,#5850,#5312,.T.);
#7107=EDGE_CURVE('',#5850,#5851,#3119,.T.);
#7108=EDGE_CURVE('',#5851,#5851,#5313,.T.);
#7109=EDGE_CURVE('',#5852,#5852,#5314,.T.);
#7110=EDGE_CURVE('',#5852,#5853,#3120,.T.);
#7111=EDGE_CURVE('',#5853,#5853,#5315,.T.);
#7112=EDGE_CURVE('',#5854,#5854,#5316,.T.);
#7113=EDGE_CURVE('',#5854,#5855,#3121,.T.);
#7114=EDGE_CURVE('',#5855,#5855,#5317,.T.);
#7115=EDGE_CURVE('',#5856,#5856,#5318,.T.);
#7116=EDGE_CURVE('',#5856,#5857,#3122,.T.);
#7117=EDGE_CURVE('',#5857,#5857,#5319,.T.);
#7118=EDGE_CURVE('',#5858,#5858,#5320,.T.);
#7119=EDGE_CURVE('',#5858,#5859,#3123,.T.);
#7120=EDGE_CURVE('',#5859,#5859,#5321,.T.);
#7121=EDGE_CURVE('',#5860,#5860,#5322,.T.);
#7122=EDGE_CURVE('',#5860,#5861,#3124,.T.);
#7123=EDGE_CURVE('',#5861,#5861,#5323,.T.);
#7124=EDGE_CURVE('',#5862,#5862,#5324,.T.);
#7125=EDGE_CURVE('',#5862,#5863,#3125,.T.);
#7126=EDGE_CURVE('',#5863,#5863,#5325,.T.);
#7127=EDGE_CURVE('',#5864,#5864,#5326,.T.);
#7128=EDGE_CURVE('',#5864,#5865,#3126,.T.);
#7129=EDGE_CURVE('',#5865,#5865,#5327,.T.);
#7130=EDGE_CURVE('',#5866,#5866,#5328,.T.);
#7131=EDGE_CURVE('',#5866,#5867,#3127,.T.);
#7132=EDGE_CURVE('',#5867,#5867,#5329,.T.);
#7133=EDGE_CURVE('',#5868,#5868,#5330,.T.);
#7134=EDGE_CURVE('',#5868,#5869,#3128,.T.);
#7135=EDGE_CURVE('',#5869,#5869,#5331,.T.);
#7136=EDGE_CURVE('',#5870,#5870,#5332,.T.);
#7137=EDGE_CURVE('',#5870,#5871,#3129,.T.);
#7138=EDGE_CURVE('',#5871,#5871,#5333,.T.);
#7139=EDGE_CURVE('',#5872,#5872,#5334,.T.);
#7140=EDGE_CURVE('',#5872,#5873,#3130,.T.);
#7141=EDGE_CURVE('',#5873,#5873,#5335,.T.);
#7142=EDGE_CURVE('',#5874,#5874,#5336,.T.);
#7143=EDGE_CURVE('',#5875,#5875,#5337,.T.);
#7144=EDGE_CURVE('',#5875,#5874,#3131,.T.);
#7145=EDGE_CURVE('',#5876,#5876,#5338,.T.);
#7146=EDGE_CURVE('',#5876,#5875,#3132,.T.);
#7147=EDGE_CURVE('',#5877,#5877,#5339,.T.);
#7148=EDGE_CURVE('',#5877,#5876,#3133,.T.);
#7149=EDGE_CURVE('',#5878,#5878,#5340,.T.);
#7150=EDGE_CURVE('',#5879,#5879,#5341,.F.);
#7151=EDGE_CURVE('',#5879,#5878,#3134,.T.);
#7152=EDGE_CURVE('',#5880,#5880,#5342,.F.);
#7153=EDGE_CURVE('',#5880,#5879,#3135,.T.);
#7154=EDGE_CURVE('',#5881,#5881,#5343,.T.);
#7155=EDGE_CURVE('',#5881,#5880,#3136,.T.);
#7156=EDGE_CURVE('',#5882,#5883,#3137,.T.);
#7157=EDGE_CURVE('',#5883,#5884,#3138,.T.);
#7158=EDGE_CURVE('',#5884,#5885,#3139,.T.);
#7159=EDGE_CURVE('',#5882,#5885,#3140,.T.);
#7160=EDGE_CURVE('',#5883,#5886,#3141,.T.);
#7161=EDGE_CURVE('',#5886,#5887,#3142,.T.);
#7162=EDGE_CURVE('',#5887,#5884,#3143,.T.);
#7163=EDGE_CURVE('',#5886,#5888,#3144,.T.);
#7164=EDGE_CURVE('',#5888,#5889,#3145,.T.);
#7165=EDGE_CURVE('',#5889,#5887,#3146,.T.);
#7166=EDGE_CURVE('',#5888,#5890,#3147,.T.);
#7167=EDGE_CURVE('',#5890,#5891,#3148,.T.);
#7168=EDGE_CURVE('',#5891,#5889,#3149,.T.);
#7169=EDGE_CURVE('',#5890,#5892,#3150,.T.);
#7170=EDGE_CURVE('',#5892,#5893,#3151,.T.);
#7171=EDGE_CURVE('',#5893,#5891,#3152,.T.);
#7172=EDGE_CURVE('',#5892,#5882,#3153,.T.);
#7173=EDGE_CURVE('',#5885,#5893,#3154,.T.);
#7174=EDGE_CURVE('',#5894,#5895,#5344,.T.);
#7175=EDGE_CURVE('',#5895,#5894,#5345,.T.);
#7176=EDGE_CURVE('',#5895,#5896,#5346,.T.);
#7177=EDGE_CURVE('',#5897,#5896,#5347,.T.);
#7178=EDGE_CURVE('',#5896,#5897,#5348,.T.);
#7179=EDGE_CURVE('',#5897,#5898,#3155,.T.);
#7180=EDGE_CURVE('',#5898,#5898,#5349,.T.);
#7181=EDGE_CURVE('',#5899,#5899,#5350,.T.);
#7182=EDGE_CURVE('',#5899,#5900,#3156,.T.);
#7183=EDGE_CURVE('',#5900,#5900,#5351,.T.);
#7184=EDGE_CURVE('',#5900,#5901,#3157,.T.);
#7185=EDGE_CURVE('',#5901,#5901,#5352,.T.);
#7186=EDGE_CURVE('',#5902,#5902,#5353,.T.);
#7187=EDGE_CURVE('',#5902,#5894,#3158,.T.);
#7188=EDGE_CURVE('',#5903,#5903,#5354,.T.);
#7189=EDGE_CURVE('',#5903,#5899,#3159,.T.);
#7190=EDGE_CURVE('',#5904,#5905,#5355,.T.);
#7191=EDGE_CURVE('',#5905,#5904,#5356,.T.);
#7192=EDGE_CURVE('',#5905,#5906,#5357,.T.);
#7193=EDGE_CURVE('',#5907,#5906,#5358,.T.);
#7194=EDGE_CURVE('',#5906,#5907,#5359,.T.);
#7195=EDGE_CURVE('',#5908,#5908,#5360,.T.);
#7196=EDGE_CURVE('',#5908,#5907,#3160,.T.);
#7197=EDGE_CURVE('',#5909,#5909,#5361,.T.);
#7198=EDGE_CURVE('',#5910,#5910,#5362,.T.);
#7199=EDGE_CURVE('',#5911,#5911,#5363,.T.);
#7200=EDGE_CURVE('',#5911,#5909,#3161,.T.);
#7201=EDGE_CURVE('',#5912,#5912,#5364,.T.);
#7202=EDGE_CURVE('',#5912,#5911,#3162,.T.);
#7203=EDGE_CURVE('',#5913,#5913,#5365,.T.);
#7204=EDGE_CURVE('',#5913,#5912,#3163,.T.);
#7205=EDGE_CURVE('',#5904,#5910,#3164,.T.);
#7206=EDGE_CURVE('',#5914,#5915,#5366,.T.);
#7207=EDGE_CURVE('',#5916,#5917,#5367,.T.);
#7208=EDGE_CURVE('',#5918,#5919,#5368,.T.);
#7209=EDGE_CURVE('',#5920,#5921,#5369,.T.);
#7210=EDGE_CURVE('',#5922,#5923,#5370,.T.);
#7211=EDGE_CURVE('',#5924,#5925,#5371,.T.);
#7212=EDGE_CURVE('',#5926,#5927,#5372,.T.);
#7213=EDGE_CURVE('',#5928,#5929,#439,.T.);
#7214=EDGE_CURVE('',#5930,#5928,#5373,.T.);
#7215=EDGE_CURVE('',#5931,#5930,#440,.T.);
#7216=EDGE_CURVE('',#5929,#5931,#5374,.T.);
#7217=EDGE_CURVE('',#5932,#5930,#5375,.T.);
#7218=EDGE_CURVE('',#5932,#5933,#441,.T.);
#7219=EDGE_CURVE('',#5934,#5933,#5376,.T.);
#7220=EDGE_CURVE('',#5934,#5935,#442,.T.);
#7221=EDGE_CURVE('',#5936,#5935,#5377,.T.);
#7222=EDGE_CURVE('',#5936,#5937,#3165,.T.);
#7223=EDGE_CURVE('',#5937,#5937,#5378,.T.);
#7224=EDGE_CURVE('',#5938,#5936,#5379,.T.);
#7225=EDGE_CURVE('',#5938,#5939,#443,.T.);
#7226=EDGE_CURVE('',#5940,#5939,#5380,.T.);
#7227=EDGE_CURVE('',#5940,#5941,#444,.T.);
#7228=EDGE_CURVE('',#5942,#5941,#5381,.T.);
#7229=EDGE_CURVE('',#5942,#5943,#445,.T.);
#7230=EDGE_CURVE('',#5944,#5943,#5382,.T.);
#7231=EDGE_CURVE('',#5944,#5945,#446,.T.);
#7232=EDGE_CURVE('',#5931,#5945,#5383,.T.);
#7233=EDGE_CURVE('',#5928,#5946,#5384,.T.);
#7234=EDGE_CURVE('',#5946,#5932,#5385,.T.);
#7235=EDGE_CURVE('',#5947,#5946,#447,.T.);
#7236=EDGE_CURVE('',#5933,#5947,#5386,.T.);
#7237=EDGE_CURVE('',#5947,#5948,#5387,.T.);
#7238=EDGE_CURVE('',#5948,#5934,#5388,.T.);
#7239=EDGE_CURVE('',#5949,#5948,#448,.T.);
#7240=EDGE_CURVE('',#5935,#5949,#5389,.T.);
#7241=EDGE_CURVE('',#5949,#5950,#5390,.T.);
#7242=EDGE_CURVE('',#5950,#5951,#5391,.T.);
#7243=EDGE_CURVE('',#5951,#5938,#5392,.T.);
#7244=EDGE_CURVE('',#5952,#5951,#449,.T.);
#7245=EDGE_CURVE('',#5939,#5952,#5393,.T.);
#7246=EDGE_CURVE('',#5952,#5953,#5394,.T.);
#7247=EDGE_CURVE('',#5953,#5940,#5395,.T.);
#7248=EDGE_CURVE('',#5954,#5953,#450,.T.);
#7249=EDGE_CURVE('',#5941,#5954,#5396,.T.);
#7250=EDGE_CURVE('',#5954,#5955,#5397,.T.);
#7251=EDGE_CURVE('',#5955,#5942,#5398,.T.);
#7252=EDGE_CURVE('',#5956,#5955,#451,.T.);
#7253=EDGE_CURVE('',#5943,#5956,#5399,.T.);
#7254=EDGE_CURVE('',#5957,#5957,#5400,.T.);
#7255=EDGE_CURVE('',#5957,#5950,#3166,.T.);
#7256=EDGE_CURVE('',#5958,#5929,#5401,.T.);
#7257=EDGE_CURVE('',#5958,#5959,#452,.T.);
#7258=EDGE_CURVE('',#5956,#5959,#5402,.T.);
#7259=EDGE_CURVE('',#5945,#5958,#5403,.T.);
#7260=EDGE_CURVE('',#5959,#5944,#5404,.T.);
#7261=EDGE_CURVE('',#5960,#5960,#5405,.T.);
#7262=EDGE_CURVE('',#5961,#5961,#5406,.T.);
#7263=EDGE_CURVE('',#5962,#5962,#5407,.T.);
#7264=EDGE_CURVE('',#5962,#5960,#3167,.T.);
#7265=EDGE_CURVE('',#5963,#5963,#5408,.T.);
#7266=EDGE_CURVE('',#5963,#5961,#3168,.T.);
#7267=EDGE_CURVE('',#5964,#5964,#5409,.T.);
#7268=EDGE_CURVE('',#5965,#5965,#5410,.T.);
#7269=EDGE_CURVE('',#5966,#5966,#5411,.T.);
#7270=EDGE_CURVE('',#5966,#5964,#3169,.T.);
#7271=EDGE_CURVE('',#5967,#5967,#5412,.T.);
#7272=EDGE_CURVE('',#5967,#5965,#3170,.T.);
#7273=EDGE_CURVE('',#5968,#5969,#3171,.T.);
#7274=EDGE_CURVE('',#5969,#5970,#3172,.T.);
#7275=EDGE_CURVE('',#5970,#5971,#3173,.T.);
#7276=EDGE_CURVE('',#5968,#5971,#3174,.T.);
#7277=EDGE_CURVE('',#5969,#5972,#3175,.T.);
#7278=EDGE_CURVE('',#5972,#5973,#3176,.T.);
#7279=EDGE_CURVE('',#5973,#5970,#3177,.T.);
#7280=EDGE_CURVE('',#5972,#5974,#3178,.T.);
#7281=EDGE_CURVE('',#5974,#5975,#3179,.T.);
#7282=EDGE_CURVE('',#5975,#5973,#3180,.T.);
#7283=EDGE_CURVE('',#5974,#5976,#3181,.T.);
#7284=EDGE_CURVE('',#5976,#5977,#3182,.T.);
#7285=EDGE_CURVE('',#5977,#5975,#3183,.T.);
#7286=EDGE_CURVE('',#5976,#5978,#3184,.T.);
#7287=EDGE_CURVE('',#5978,#5979,#3185,.T.);
#7288=EDGE_CURVE('',#5979,#5977,#3186,.T.);
#7289=EDGE_CURVE('',#5978,#5968,#3187,.T.);
#7290=EDGE_CURVE('',#5971,#5979,#3188,.T.);
#7291=EDGE_CURVE('',#5980,#5980,#5413,.T.);
#7292=EDGE_CURVE('',#5981,#5981,#5414,.T.);
#7293=EDGE_CURVE('',#5982,#5982,#5415,.T.);
#7294=EDGE_CURVE('',#5982,#5981,#3189,.T.);
#7295=EDGE_CURVE('',#5983,#5983,#5416,.T.);
#7296=EDGE_CURVE('',#5983,#5982,#3190,.T.);
#7297=EDGE_CURVE('',#5984,#5984,#5417,.T.);
#7298=EDGE_CURVE('',#5984,#5983,#3191,.T.);
#7299=EDGE_CURVE('',#5985,#5985,#5418,.T.);
#7300=EDGE_CURVE('',#5986,#5986,#5419,.F.);
#7301=EDGE_CURVE('',#5986,#5985,#3192,.T.);
#7302=EDGE_CURVE('',#5980,#5986,#3193,.T.);
#7303=EDGE_CURVE('',#5987,#5987,#5420,.T.);
#7304=EDGE_CURVE('',#5987,#5988,#3194,.T.);
#7305=EDGE_CURVE('',#5988,#5988,#5421,.T.);
#7306=EDGE_CURVE('',#5989,#5990,#3195,.T.);
#7307=EDGE_CURVE('',#5991,#5989,#3196,.T.);
#7308=EDGE_CURVE('',#5992,#5991,#3197,.T.);
#7309=EDGE_CURVE('',#5992,#5990,#3198,.T.);
#7310=EDGE_CURVE('',#5993,#5994,#3199,.T.);
#7311=EDGE_CURVE('',#5993,#5995,#3200,.T.);
#7312=EDGE_CURVE('',#5996,#5995,#3201,.T.);
#7313=EDGE_CURVE('',#5994,#5996,#3202,.T.);
#7314=EDGE_CURVE('',#5990,#5997,#5422,.T.);
#7315=EDGE_CURVE('',#5998,#5992,#3203,.T.);
#7316=EDGE_CURVE('',#5998,#5999,#3204,.T.);
#7317=EDGE_CURVE('',#5995,#5999,#3205,.T.);
#7318=EDGE_CURVE('',#5997,#5993,#5423,.T.);
#7319=EDGE_CURVE('',#5994,#6000,#5424,.T.);
#7320=EDGE_CURVE('',#6001,#5996,#3206,.T.);
#7321=EDGE_CURVE('',#6002,#6001,#3207,.T.);
#7322=EDGE_CURVE('',#5991,#6002,#3208,.T.);
#7323=EDGE_CURVE('',#6000,#5989,#5425,.T.);
#7324=EDGE_CURVE('',#6002,#6003,#3209,.T.);
#7325=EDGE_CURVE('',#6004,#6001,#3210,.T.);
#7326=EDGE_CURVE('',#6003,#6004,#3211,.T.);
#7327=EDGE_CURVE('',#6003,#6005,#3212,.T.);
#7328=EDGE_CURVE('',#6006,#6004,#3213,.T.);
#7329=EDGE_CURVE('',#6005,#6006,#3214,.T.);
#7330=EDGE_CURVE('',#6005,#6007,#3215,.T.);
#7331=EDGE_CURVE('',#6008,#6006,#3216,.T.);
#7332=EDGE_CURVE('',#6007,#6008,#3217,.T.);
#7333=EDGE_CURVE('',#6007,#6009,#3218,.T.);
#7334=EDGE_CURVE('',#6010,#6008,#3219,.T.);
#7335=EDGE_CURVE('',#6009,#6010,#3220,.T.);
#7336=EDGE_CURVE('',#6009,#6011,#3221,.T.);
#7337=EDGE_CURVE('',#6012,#6010,#3222,.T.);
#7338=EDGE_CURVE('',#6011,#6012,#3223,.T.);
#7339=EDGE_CURVE('',#6011,#6013,#3224,.T.);
#7340=EDGE_CURVE('',#6014,#6012,#3225,.T.);
#7341=EDGE_CURVE('',#6013,#6014,#3226,.T.);
#7342=EDGE_CURVE('',#6013,#6015,#3227,.T.);
#7343=EDGE_CURVE('',#6016,#6014,#3228,.T.);
#7344=EDGE_CURVE('',#6015,#6016,#3229,.T.);
#7345=EDGE_CURVE('',#6015,#6017,#3230,.T.);
#7346=EDGE_CURVE('',#6018,#6016,#3231,.T.);
#7347=EDGE_CURVE('',#6017,#6018,#3232,.T.);
#7348=EDGE_CURVE('',#6017,#6019,#3233,.T.);
#7349=EDGE_CURVE('',#6020,#6018,#3234,.T.);
#7350=EDGE_CURVE('',#6019,#6020,#3235,.T.);
#7351=EDGE_CURVE('',#6019,#6021,#3236,.T.);
#7352=EDGE_CURVE('',#6022,#6020,#3237,.T.);
#7353=EDGE_CURVE('',#6021,#6022,#3238,.T.);
#7354=EDGE_CURVE('',#6021,#6023,#3239,.T.);
#7355=EDGE_CURVE('',#6024,#6022,#3240,.T.);
#7356=EDGE_CURVE('',#6023,#6024,#3241,.T.);
#7357=EDGE_CURVE('',#6023,#6025,#3242,.T.);
#7358=EDGE_CURVE('',#6026,#6024,#3243,.T.);
#7359=EDGE_CURVE('',#6025,#6026,#3244,.T.);
#7360=EDGE_CURVE('',#6025,#6027,#3245,.T.);
#7361=EDGE_CURVE('',#6028,#6026,#3246,.T.);
#7362=EDGE_CURVE('',#6027,#6028,#3247,.T.);
#7363=EDGE_CURVE('',#6027,#6029,#3248,.T.);
#7364=EDGE_CURVE('',#6030,#6028,#3249,.T.);
#7365=EDGE_CURVE('',#6029,#6030,#3250,.T.);
#7366=EDGE_CURVE('',#6029,#6031,#3251,.T.);
#7367=EDGE_CURVE('',#6032,#6030,#3252,.T.);
#7368=EDGE_CURVE('',#6031,#6032,#3253,.T.);
#7369=EDGE_CURVE('',#6031,#6033,#3254,.T.);
#7370=EDGE_CURVE('',#6034,#6032,#3255,.T.);
#7371=EDGE_CURVE('',#6033,#6034,#3256,.T.);
#7372=EDGE_CURVE('',#6033,#6035,#3257,.T.);
#7373=EDGE_CURVE('',#6036,#6034,#3258,.T.);
#7374=EDGE_CURVE('',#6035,#6036,#3259,.T.);
#7375=EDGE_CURVE('',#6035,#6037,#3260,.T.);
#7376=EDGE_CURVE('',#6038,#6036,#3261,.T.);
#7377=EDGE_CURVE('',#6037,#6038,#3262,.T.);
#7378=EDGE_CURVE('',#6037,#6039,#3263,.T.);
#7379=EDGE_CURVE('',#6040,#6038,#3264,.T.);
#7380=EDGE_CURVE('',#6039,#6040,#3265,.T.);
#7381=EDGE_CURVE('',#6039,#6041,#3266,.T.);
#7382=EDGE_CURVE('',#6042,#6040,#3267,.T.);
#7383=EDGE_CURVE('',#6041,#6042,#3268,.T.);
#7384=EDGE_CURVE('',#6041,#6043,#3269,.T.);
#7385=EDGE_CURVE('',#6044,#6042,#3270,.T.);
#7386=EDGE_CURVE('',#6043,#6044,#3271,.T.);
#7387=EDGE_CURVE('',#6043,#6045,#3272,.T.);
#7388=EDGE_CURVE('',#6046,#6044,#3273,.T.);
#7389=EDGE_CURVE('',#6045,#6046,#3274,.T.);
#7390=EDGE_CURVE('',#6045,#6047,#3275,.T.);
#7391=EDGE_CURVE('',#6048,#6046,#3276,.T.);
#7392=EDGE_CURVE('',#6047,#6048,#3277,.T.);
#7393=EDGE_CURVE('',#6047,#6049,#3278,.T.);
#7394=EDGE_CURVE('',#6050,#6048,#3279,.T.);
#7395=EDGE_CURVE('',#6049,#6050,#3280,.T.);
#7396=EDGE_CURVE('',#6049,#6051,#3281,.T.);
#7397=EDGE_CURVE('',#6052,#6050,#3282,.T.);
#7398=EDGE_CURVE('',#6051,#6052,#3283,.T.);
#7399=EDGE_CURVE('',#6051,#6053,#3284,.T.);
#7400=EDGE_CURVE('',#6054,#6052,#3285,.T.);
#7401=EDGE_CURVE('',#6053,#6054,#3286,.T.);
#7402=EDGE_CURVE('',#6053,#6055,#3287,.T.);
#7403=EDGE_CURVE('',#6056,#6054,#3288,.T.);
#7404=EDGE_CURVE('',#6055,#6056,#3289,.T.);
#7405=EDGE_CURVE('',#6055,#6057,#3290,.T.);
#7406=EDGE_CURVE('',#6058,#6056,#3291,.T.);
#7407=EDGE_CURVE('',#6057,#6058,#3292,.T.);
#7408=EDGE_CURVE('',#6057,#6059,#3293,.T.);
#7409=EDGE_CURVE('',#6060,#6058,#3294,.T.);
#7410=EDGE_CURVE('',#6059,#6060,#3295,.T.);
#7411=EDGE_CURVE('',#6059,#6061,#3296,.T.);
#7412=EDGE_CURVE('',#6062,#6060,#3297,.T.);
#7413=EDGE_CURVE('',#6061,#6062,#3298,.T.);
#7414=EDGE_CURVE('',#6061,#6063,#3299,.T.);
#7415=EDGE_CURVE('',#6064,#6062,#3300,.T.);
#7416=EDGE_CURVE('',#6063,#6064,#3301,.T.);
#7417=EDGE_CURVE('',#6063,#6065,#3302,.T.);
#7418=EDGE_CURVE('',#6066,#6064,#3303,.T.);
#7419=EDGE_CURVE('',#6065,#6066,#3304,.T.);
#7420=EDGE_CURVE('',#6065,#6067,#3305,.T.);
#7421=EDGE_CURVE('',#6068,#6066,#3306,.T.);
#7422=EDGE_CURVE('',#6067,#6068,#3307,.T.);
#7423=EDGE_CURVE('',#6067,#6069,#3308,.T.);
#7424=EDGE_CURVE('',#6070,#6068,#3309,.T.);
#7425=EDGE_CURVE('',#6069,#6070,#3310,.T.);
#7426=EDGE_CURVE('',#6069,#6071,#3311,.T.);
#7427=EDGE_CURVE('',#6072,#6070,#3312,.T.);
#7428=EDGE_CURVE('',#6071,#6072,#3313,.T.);
#7429=EDGE_CURVE('',#6071,#6073,#3314,.T.);
#7430=EDGE_CURVE('',#6074,#6072,#3315,.T.);
#7431=EDGE_CURVE('',#6073,#6074,#3316,.T.);
#7432=EDGE_CURVE('',#6073,#6075,#3317,.T.);
#7433=EDGE_CURVE('',#6076,#6074,#3318,.T.);
#7434=EDGE_CURVE('',#6075,#6076,#3319,.T.);
#7435=EDGE_CURVE('',#6075,#6077,#3320,.T.);
#7436=EDGE_CURVE('',#6078,#6076,#3321,.T.);
#7437=EDGE_CURVE('',#6077,#6078,#3322,.T.);
#7438=EDGE_CURVE('',#6077,#6079,#3323,.T.);
#7439=EDGE_CURVE('',#6080,#6078,#3324,.T.);
#7440=EDGE_CURVE('',#6079,#6080,#3325,.T.);
#7441=EDGE_CURVE('',#6079,#6081,#3326,.T.);
#7442=EDGE_CURVE('',#6082,#6080,#3327,.T.);
#7443=EDGE_CURVE('',#6081,#6082,#3328,.T.);
#7444=EDGE_CURVE('',#6081,#6083,#3329,.T.);
#7445=EDGE_CURVE('',#6084,#6082,#3330,.T.);
#7446=EDGE_CURVE('',#6083,#6084,#3331,.T.);
#7447=EDGE_CURVE('',#6083,#6085,#3332,.T.);
#7448=EDGE_CURVE('',#6086,#6084,#3333,.T.);
#7449=EDGE_CURVE('',#6085,#6086,#3334,.T.);
#7450=EDGE_CURVE('',#6085,#6087,#3335,.T.);
#7451=EDGE_CURVE('',#6088,#6086,#3336,.T.);
#7452=EDGE_CURVE('',#6087,#6088,#3337,.T.);
#7453=EDGE_CURVE('',#6087,#6089,#3338,.T.);
#7454=EDGE_CURVE('',#6090,#6088,#3339,.T.);
#7455=EDGE_CURVE('',#6089,#6090,#3340,.T.);
#7456=EDGE_CURVE('',#6089,#6091,#3341,.T.);
#7457=EDGE_CURVE('',#6092,#6090,#3342,.T.);
#7458=EDGE_CURVE('',#6091,#6092,#3343,.T.);
#7459=EDGE_CURVE('',#6091,#6093,#3344,.T.);
#7460=EDGE_CURVE('',#6094,#6092,#3345,.T.);
#7461=EDGE_CURVE('',#6093,#6094,#3346,.T.);
#7462=EDGE_CURVE('',#6093,#6095,#3347,.T.);
#7463=EDGE_CURVE('',#6096,#6094,#3348,.T.);
#7464=EDGE_CURVE('',#6095,#6096,#3349,.T.);
#7465=EDGE_CURVE('',#6095,#6097,#3350,.T.);
#7466=EDGE_CURVE('',#6098,#6096,#3351,.T.);
#7467=EDGE_CURVE('',#6097,#6098,#3352,.T.);
#7468=EDGE_CURVE('',#6097,#6099,#3353,.T.);
#7469=EDGE_CURVE('',#6100,#6098,#3354,.T.);
#7470=EDGE_CURVE('',#6099,#6100,#3355,.T.);
#7471=EDGE_CURVE('',#6099,#6101,#3356,.T.);
#7472=EDGE_CURVE('',#6102,#6100,#3357,.T.);
#7473=EDGE_CURVE('',#6101,#6102,#3358,.T.);
#7474=EDGE_CURVE('',#6101,#6103,#3359,.T.);
#7475=EDGE_CURVE('',#6104,#6102,#3360,.T.);
#7476=EDGE_CURVE('',#6103,#6104,#3361,.T.);
#7477=EDGE_CURVE('',#6103,#6105,#3362,.T.);
#7478=EDGE_CURVE('',#6106,#6104,#3363,.T.);
#7479=EDGE_CURVE('',#6105,#6106,#3364,.T.);
#7480=EDGE_CURVE('',#6105,#6107,#3365,.T.);
#7481=EDGE_CURVE('',#6108,#6106,#3366,.T.);
#7482=EDGE_CURVE('',#6107,#6108,#3367,.T.);
#7483=EDGE_CURVE('',#6107,#6109,#3368,.T.);
#7484=EDGE_CURVE('',#6110,#6108,#3369,.T.);
#7485=EDGE_CURVE('',#6109,#6110,#3370,.T.);
#7486=EDGE_CURVE('',#6109,#6111,#3371,.T.);
#7487=EDGE_CURVE('',#6112,#6110,#3372,.T.);
#7488=EDGE_CURVE('',#6111,#6112,#3373,.T.);
#7489=EDGE_CURVE('',#6111,#6113,#3374,.T.);
#7490=EDGE_CURVE('',#6114,#6112,#3375,.T.);
#7491=EDGE_CURVE('',#6113,#6114,#3376,.T.);
#7492=EDGE_CURVE('',#6113,#6115,#3377,.T.);
#7493=EDGE_CURVE('',#6116,#6114,#3378,.T.);
#7494=EDGE_CURVE('',#6115,#6116,#3379,.T.);
#7495=EDGE_CURVE('',#6115,#6117,#3380,.T.);
#7496=EDGE_CURVE('',#6118,#6116,#3381,.T.);
#7497=EDGE_CURVE('',#6117,#6118,#3382,.T.);
#7498=EDGE_CURVE('',#6117,#6119,#3383,.T.);
#7499=EDGE_CURVE('',#6120,#6118,#3384,.T.);
#7500=EDGE_CURVE('',#6119,#6120,#3385,.T.);
#7501=EDGE_CURVE('',#6119,#6121,#3386,.T.);
#7502=EDGE_CURVE('',#6122,#6120,#3387,.T.);
#7503=EDGE_CURVE('',#6121,#6122,#3388,.T.);
#7504=EDGE_CURVE('',#6121,#6123,#3389,.T.);
#7505=EDGE_CURVE('',#6124,#6122,#3390,.T.);
#7506=EDGE_CURVE('',#6123,#6124,#3391,.T.);
#7507=EDGE_CURVE('',#6123,#6125,#3392,.T.);
#7508=EDGE_CURVE('',#6126,#6124,#3393,.T.);
#7509=EDGE_CURVE('',#6125,#6126,#3394,.T.);
#7510=EDGE_CURVE('',#6125,#6127,#3395,.T.);
#7511=EDGE_CURVE('',#6128,#6126,#3396,.T.);
#7512=EDGE_CURVE('',#6127,#6128,#3397,.T.);
#7513=EDGE_CURVE('',#6127,#6129,#3398,.T.);
#7514=EDGE_CURVE('',#6130,#6128,#3399,.T.);
#7515=EDGE_CURVE('',#6129,#6130,#3400,.T.);
#7516=EDGE_CURVE('',#6129,#6131,#3401,.T.);
#7517=EDGE_CURVE('',#6132,#6130,#3402,.T.);
#7518=EDGE_CURVE('',#6131,#6132,#3403,.T.);
#7519=EDGE_CURVE('',#6131,#6133,#3404,.T.);
#7520=EDGE_CURVE('',#6134,#6132,#3405,.T.);
#7521=EDGE_CURVE('',#6133,#6134,#3406,.T.);
#7522=EDGE_CURVE('',#6133,#6135,#3407,.T.);
#7523=EDGE_CURVE('',#6136,#6134,#3408,.T.);
#7524=EDGE_CURVE('',#6135,#6136,#3409,.T.);
#7525=EDGE_CURVE('',#6135,#6137,#3410,.T.);
#7526=EDGE_CURVE('',#6138,#6136,#3411,.T.);
#7527=EDGE_CURVE('',#6137,#6138,#3412,.T.);
#7528=EDGE_CURVE('',#6137,#6139,#3413,.T.);
#7529=EDGE_CURVE('',#6140,#6138,#3414,.T.);
#7530=EDGE_CURVE('',#6139,#6140,#3415,.T.);
#7531=EDGE_CURVE('',#6139,#6141,#3416,.T.);
#7532=EDGE_CURVE('',#6142,#6140,#3417,.T.);
#7533=EDGE_CURVE('',#6141,#6142,#3418,.T.);
#7534=EDGE_CURVE('',#6141,#6143,#3419,.T.);
#7535=EDGE_CURVE('',#6144,#6142,#3420,.T.);
#7536=EDGE_CURVE('',#6143,#6144,#3421,.T.);
#7537=EDGE_CURVE('',#6143,#6145,#3422,.T.);
#7538=EDGE_CURVE('',#6146,#6144,#3423,.T.);
#7539=EDGE_CURVE('',#6145,#6146,#3424,.T.);
#7540=EDGE_CURVE('',#6145,#6147,#3425,.T.);
#7541=EDGE_CURVE('',#6148,#6146,#3426,.T.);
#7542=EDGE_CURVE('',#6147,#6148,#3427,.T.);
#7543=EDGE_CURVE('',#6147,#6149,#3428,.T.);
#7544=EDGE_CURVE('',#6150,#6148,#3429,.T.);
#7545=EDGE_CURVE('',#6149,#6150,#3430,.T.);
#7546=EDGE_CURVE('',#6149,#6151,#3431,.T.);
#7547=EDGE_CURVE('',#6152,#6150,#3432,.T.);
#7548=EDGE_CURVE('',#6151,#6152,#3433,.T.);
#7549=EDGE_CURVE('',#6151,#6153,#3434,.T.);
#7550=EDGE_CURVE('',#6154,#6152,#3435,.T.);
#7551=EDGE_CURVE('',#6153,#6154,#3436,.T.);
#7552=EDGE_CURVE('',#6153,#6155,#3437,.T.);
#7553=EDGE_CURVE('',#6156,#6154,#3438,.T.);
#7554=EDGE_CURVE('',#6155,#6156,#3439,.T.);
#7555=EDGE_CURVE('',#6155,#6157,#3440,.T.);
#7556=EDGE_CURVE('',#6158,#6156,#3441,.T.);
#7557=EDGE_CURVE('',#6157,#6158,#3442,.T.);
#7558=EDGE_CURVE('',#6157,#6159,#3443,.T.);
#7559=EDGE_CURVE('',#6160,#6158,#3444,.T.);
#7560=EDGE_CURVE('',#6159,#6160,#3445,.T.);
#7561=EDGE_CURVE('',#6159,#6161,#3446,.T.);
#7562=EDGE_CURVE('',#6162,#6160,#3447,.T.);
#7563=EDGE_CURVE('',#6161,#6162,#3448,.T.);
#7564=EDGE_CURVE('',#6161,#6163,#3449,.T.);
#7565=EDGE_CURVE('',#6164,#6162,#3450,.T.);
#7566=EDGE_CURVE('',#6163,#6164,#3451,.T.);
#7567=EDGE_CURVE('',#6163,#6165,#3452,.T.);
#7568=EDGE_CURVE('',#6166,#6164,#3453,.T.);
#7569=EDGE_CURVE('',#6165,#6166,#3454,.T.);
#7570=EDGE_CURVE('',#6165,#6167,#3455,.T.);
#7571=EDGE_CURVE('',#6168,#6166,#3456,.T.);
#7572=EDGE_CURVE('',#6167,#6168,#3457,.T.);
#7573=EDGE_CURVE('',#6167,#6169,#3458,.T.);
#7574=EDGE_CURVE('',#6170,#6168,#3459,.T.);
#7575=EDGE_CURVE('',#6169,#6170,#3460,.T.);
#7576=EDGE_CURVE('',#6169,#6171,#3461,.T.);
#7577=EDGE_CURVE('',#6172,#6170,#3462,.T.);
#7578=EDGE_CURVE('',#6171,#6172,#3463,.T.);
#7579=EDGE_CURVE('',#6171,#6173,#3464,.T.);
#7580=EDGE_CURVE('',#6174,#6172,#3465,.T.);
#7581=EDGE_CURVE('',#6173,#6174,#3466,.T.);
#7582=EDGE_CURVE('',#6173,#6175,#3467,.T.);
#7583=EDGE_CURVE('',#6176,#6174,#3468,.T.);
#7584=EDGE_CURVE('',#6175,#6176,#3469,.T.);
#7585=EDGE_CURVE('',#6175,#6177,#3470,.T.);
#7586=EDGE_CURVE('',#6178,#6176,#3471,.T.);
#7587=EDGE_CURVE('',#6177,#6178,#3472,.T.);
#7588=EDGE_CURVE('',#6177,#6179,#3473,.T.);
#7589=EDGE_CURVE('',#6180,#6178,#3474,.T.);
#7590=EDGE_CURVE('',#6179,#6180,#3475,.T.);
#7591=EDGE_CURVE('',#6179,#6181,#3476,.T.);
#7592=EDGE_CURVE('',#6182,#6180,#3477,.T.);
#7593=EDGE_CURVE('',#6181,#6182,#3478,.T.);
#7594=EDGE_CURVE('',#6181,#6183,#3479,.T.);
#7595=EDGE_CURVE('',#6184,#6182,#3480,.T.);
#7596=EDGE_CURVE('',#6183,#6184,#3481,.T.);
#7597=EDGE_CURVE('',#6183,#6185,#3482,.T.);
#7598=EDGE_CURVE('',#6186,#6184,#3483,.T.);
#7599=EDGE_CURVE('',#6185,#6186,#3484,.T.);
#7600=EDGE_CURVE('',#6185,#6187,#3485,.T.);
#7601=EDGE_CURVE('',#6188,#6186,#3486,.T.);
#7602=EDGE_CURVE('',#6187,#6188,#3487,.T.);
#7603=EDGE_CURVE('',#6187,#6189,#3488,.T.);
#7604=EDGE_CURVE('',#6190,#6188,#3489,.T.);
#7605=EDGE_CURVE('',#6189,#6190,#3490,.T.);
#7606=EDGE_CURVE('',#6189,#6191,#3491,.T.);
#7607=EDGE_CURVE('',#6192,#6190,#3492,.T.);
#7608=EDGE_CURVE('',#6191,#6192,#3493,.T.);
#7609=EDGE_CURVE('',#6191,#6193,#3494,.T.);
#7610=EDGE_CURVE('',#6194,#6192,#3495,.T.);
#7611=EDGE_CURVE('',#6193,#6194,#3496,.T.);
#7612=EDGE_CURVE('',#6193,#6195,#3497,.T.);
#7613=EDGE_CURVE('',#6196,#6194,#3498,.T.);
#7614=EDGE_CURVE('',#6195,#6196,#3499,.T.);
#7615=EDGE_CURVE('',#6195,#6197,#3500,.T.);
#7616=EDGE_CURVE('',#6198,#6196,#3501,.T.);
#7617=EDGE_CURVE('',#6197,#6198,#3502,.T.);
#7618=EDGE_CURVE('',#6197,#6199,#3503,.T.);
#7619=EDGE_CURVE('',#6200,#6198,#3504,.T.);
#7620=EDGE_CURVE('',#6199,#6200,#3505,.T.);
#7621=EDGE_CURVE('',#6199,#6201,#3506,.T.);
#7622=EDGE_CURVE('',#6202,#6200,#3507,.T.);
#7623=EDGE_CURVE('',#6201,#6202,#3508,.T.);
#7624=EDGE_CURVE('',#6201,#6203,#3509,.T.);
#7625=EDGE_CURVE('',#6204,#6202,#3510,.T.);
#7626=EDGE_CURVE('',#6203,#6204,#3511,.T.);
#7627=EDGE_CURVE('',#6203,#6205,#3512,.T.);
#7628=EDGE_CURVE('',#6206,#6204,#3513,.T.);
#7629=EDGE_CURVE('',#6205,#6206,#3514,.T.);
#7630=EDGE_CURVE('',#6205,#6207,#3515,.T.);
#7631=EDGE_CURVE('',#6208,#6206,#3516,.T.);
#7632=EDGE_CURVE('',#6207,#6208,#3517,.T.);
#7633=EDGE_CURVE('',#6207,#6209,#3518,.T.);
#7634=EDGE_CURVE('',#6210,#6208,#3519,.T.);
#7635=EDGE_CURVE('',#6209,#6210,#3520,.T.);
#7636=EDGE_CURVE('',#6209,#6211,#3521,.T.);
#7637=EDGE_CURVE('',#6212,#6210,#3522,.T.);
#7638=EDGE_CURVE('',#6211,#6212,#3523,.T.);
#7639=EDGE_CURVE('',#6211,#6213,#3524,.T.);
#7640=EDGE_CURVE('',#6214,#6212,#3525,.T.);
#7641=EDGE_CURVE('',#6213,#6214,#3526,.T.);
#7642=EDGE_CURVE('',#6213,#6215,#3527,.T.);
#7643=EDGE_CURVE('',#6216,#6214,#3528,.T.);
#7644=EDGE_CURVE('',#6215,#6216,#3529,.T.);
#7645=EDGE_CURVE('',#6215,#6217,#3530,.T.);
#7646=EDGE_CURVE('',#6218,#6216,#3531,.T.);
#7647=EDGE_CURVE('',#6217,#6218,#3532,.T.);
#7648=EDGE_CURVE('',#6217,#6219,#3533,.T.);
#7649=EDGE_CURVE('',#6220,#6218,#3534,.T.);
#7650=EDGE_CURVE('',#6219,#6220,#3535,.T.);
#7651=EDGE_CURVE('',#6219,#6221,#3536,.T.);
#7652=EDGE_CURVE('',#6222,#6220,#3537,.T.);
#7653=EDGE_CURVE('',#6221,#6222,#3538,.T.);
#7654=EDGE_CURVE('',#6221,#6223,#3539,.T.);
#7655=EDGE_CURVE('',#6224,#6222,#3540,.T.);
#7656=EDGE_CURVE('',#6223,#6224,#3541,.T.);
#7657=EDGE_CURVE('',#6223,#6225,#3542,.T.);
#7658=EDGE_CURVE('',#6226,#6224,#3543,.T.);
#7659=EDGE_CURVE('',#6225,#6226,#3544,.T.);
#7660=EDGE_CURVE('',#6225,#6227,#3545,.T.);
#7661=EDGE_CURVE('',#6228,#6226,#3546,.T.);
#7662=EDGE_CURVE('',#6227,#6228,#3547,.T.);
#7663=EDGE_CURVE('',#6227,#6229,#3548,.T.);
#7664=EDGE_CURVE('',#6230,#6228,#3549,.T.);
#7665=EDGE_CURVE('',#6229,#6230,#3550,.T.);
#7666=EDGE_CURVE('',#6229,#6231,#3551,.T.);
#7667=EDGE_CURVE('',#6232,#6230,#3552,.T.);
#7668=EDGE_CURVE('',#6231,#6232,#3553,.T.);
#7669=EDGE_CURVE('',#6231,#6233,#3554,.T.);
#7670=EDGE_CURVE('',#6234,#6232,#3555,.T.);
#7671=EDGE_CURVE('',#6233,#6234,#3556,.T.);
#7672=EDGE_CURVE('',#6233,#6235,#3557,.T.);
#7673=EDGE_CURVE('',#6236,#6234,#3558,.T.);
#7674=EDGE_CURVE('',#6235,#6236,#3559,.T.);
#7675=EDGE_CURVE('',#6235,#6237,#3560,.T.);
#7676=EDGE_CURVE('',#6238,#6236,#3561,.T.);
#7677=EDGE_CURVE('',#6237,#6238,#3562,.T.);
#7678=EDGE_CURVE('',#6237,#6239,#3563,.T.);
#7679=EDGE_CURVE('',#6240,#6238,#3564,.T.);
#7680=EDGE_CURVE('',#6239,#6240,#3565,.T.);
#7681=EDGE_CURVE('',#6239,#6241,#3566,.T.);
#7682=EDGE_CURVE('',#6242,#6240,#3567,.T.);
#7683=EDGE_CURVE('',#6241,#6242,#3568,.T.);
#7684=EDGE_CURVE('',#6241,#6243,#3569,.T.);
#7685=EDGE_CURVE('',#6244,#6242,#3570,.T.);
#7686=EDGE_CURVE('',#6243,#6244,#3571,.T.);
#7687=EDGE_CURVE('',#6243,#6245,#3572,.T.);
#7688=EDGE_CURVE('',#6246,#6244,#3573,.T.);
#7689=EDGE_CURVE('',#6245,#6246,#3574,.T.);
#7690=EDGE_CURVE('',#6245,#6247,#3575,.T.);
#7691=EDGE_CURVE('',#6248,#6246,#3576,.T.);
#7692=EDGE_CURVE('',#6247,#6248,#3577,.T.);
#7693=EDGE_CURVE('',#6247,#6249,#3578,.T.);
#7694=EDGE_CURVE('',#6250,#6248,#3579,.T.);
#7695=EDGE_CURVE('',#6249,#6250,#3580,.T.);
#7696=EDGE_CURVE('',#6249,#6251,#3581,.T.);
#7697=EDGE_CURVE('',#6252,#6250,#3582,.T.);
#7698=EDGE_CURVE('',#6251,#6252,#3583,.T.);
#7699=EDGE_CURVE('',#6251,#6253,#3584,.T.);
#7700=EDGE_CURVE('',#6254,#6252,#3585,.T.);
#7701=EDGE_CURVE('',#6253,#6254,#3586,.T.);
#7702=EDGE_CURVE('',#6253,#6255,#3587,.T.);
#7703=EDGE_CURVE('',#6256,#6254,#3588,.T.);
#7704=EDGE_CURVE('',#6255,#6256,#3589,.T.);
#7705=EDGE_CURVE('',#6255,#6257,#3590,.T.);
#7706=EDGE_CURVE('',#6258,#6256,#3591,.T.);
#7707=EDGE_CURVE('',#6257,#6258,#3592,.T.);
#7708=EDGE_CURVE('',#6257,#6259,#3593,.T.);
#7709=EDGE_CURVE('',#6260,#6258,#3594,.T.);
#7710=EDGE_CURVE('',#6259,#6260,#3595,.T.);
#7711=EDGE_CURVE('',#6259,#6261,#3596,.T.);
#7712=EDGE_CURVE('',#6262,#6260,#3597,.T.);
#7713=EDGE_CURVE('',#6261,#6262,#3598,.T.);
#7714=EDGE_CURVE('',#6261,#6263,#3599,.T.);
#7715=EDGE_CURVE('',#6264,#6262,#3600,.T.);
#7716=EDGE_CURVE('',#6263,#6264,#3601,.T.);
#7717=EDGE_CURVE('',#6263,#6265,#3602,.T.);
#7718=EDGE_CURVE('',#6266,#6264,#3603,.T.);
#7719=EDGE_CURVE('',#6265,#6266,#3604,.T.);
#7720=EDGE_CURVE('',#6265,#6267,#3605,.T.);
#7721=EDGE_CURVE('',#6268,#6266,#3606,.T.);
#7722=EDGE_CURVE('',#6267,#6268,#3607,.T.);
#7723=EDGE_CURVE('',#6267,#6269,#3608,.T.);
#7724=EDGE_CURVE('',#6270,#6268,#3609,.T.);
#7725=EDGE_CURVE('',#6269,#6270,#3610,.T.);
#7726=EDGE_CURVE('',#6269,#6271,#3611,.T.);
#7727=EDGE_CURVE('',#6272,#6270,#3612,.T.);
#7728=EDGE_CURVE('',#6271,#6272,#3613,.T.);
#7729=EDGE_CURVE('',#6271,#6273,#3614,.T.);
#7730=EDGE_CURVE('',#6274,#6272,#3615,.T.);
#7731=EDGE_CURVE('',#6273,#6274,#3616,.T.);
#7732=EDGE_CURVE('',#6273,#6275,#3617,.T.);
#7733=EDGE_CURVE('',#6276,#6274,#3618,.T.);
#7734=EDGE_CURVE('',#6275,#6276,#3619,.T.);
#7735=EDGE_CURVE('',#6275,#6277,#3620,.T.);
#7736=EDGE_CURVE('',#6278,#6276,#3621,.T.);
#7737=EDGE_CURVE('',#6277,#6278,#3622,.T.);
#7738=EDGE_CURVE('',#6277,#6279,#3623,.T.);
#7739=EDGE_CURVE('',#6280,#6278,#3624,.T.);
#7740=EDGE_CURVE('',#6279,#6280,#3625,.T.);
#7741=EDGE_CURVE('',#6279,#6281,#3626,.T.);
#7742=EDGE_CURVE('',#6282,#6280,#3627,.T.);
#7743=EDGE_CURVE('',#6281,#6282,#3628,.T.);
#7744=EDGE_CURVE('',#6281,#6283,#3629,.T.);
#7745=EDGE_CURVE('',#6284,#6282,#3630,.T.);
#7746=EDGE_CURVE('',#6283,#6284,#3631,.T.);
#7747=EDGE_CURVE('',#6283,#6285,#3632,.T.);
#7748=EDGE_CURVE('',#6286,#6284,#3633,.T.);
#7749=EDGE_CURVE('',#6285,#6286,#3634,.T.);
#7750=EDGE_CURVE('',#6285,#6287,#3635,.T.);
#7751=EDGE_CURVE('',#6288,#6286,#3636,.T.);
#7752=EDGE_CURVE('',#6287,#6288,#3637,.T.);
#7753=EDGE_CURVE('',#6287,#6289,#3638,.T.);
#7754=EDGE_CURVE('',#6290,#6288,#3639,.T.);
#7755=EDGE_CURVE('',#6289,#6290,#3640,.T.);
#7756=EDGE_CURVE('',#6289,#6291,#3641,.T.);
#7757=EDGE_CURVE('',#6292,#6290,#3642,.T.);
#7758=EDGE_CURVE('',#6291,#6292,#3643,.T.);
#7759=EDGE_CURVE('',#6291,#6293,#3644,.T.);
#7760=EDGE_CURVE('',#6294,#6292,#3645,.T.);
#7761=EDGE_CURVE('',#6293,#6294,#3646,.T.);
#7762=EDGE_CURVE('',#6293,#6295,#3647,.T.);
#7763=EDGE_CURVE('',#6296,#6294,#3648,.T.);
#7764=EDGE_CURVE('',#6295,#6296,#3649,.T.);
#7765=EDGE_CURVE('',#6295,#6297,#3650,.T.);
#7766=EDGE_CURVE('',#6298,#6296,#3651,.T.);
#7767=EDGE_CURVE('',#6297,#6298,#3652,.T.);
#7768=EDGE_CURVE('',#6297,#6299,#3653,.T.);
#7769=EDGE_CURVE('',#6300,#6298,#3654,.T.);
#7770=EDGE_CURVE('',#6299,#6300,#3655,.T.);
#7771=EDGE_CURVE('',#6299,#6301,#3656,.T.);
#7772=EDGE_CURVE('',#6302,#6300,#3657,.T.);
#7773=EDGE_CURVE('',#6301,#6302,#3658,.T.);
#7774=EDGE_CURVE('',#6301,#6303,#3659,.T.);
#7775=EDGE_CURVE('',#6304,#6302,#3660,.T.);
#7776=EDGE_CURVE('',#6303,#6304,#3661,.T.);
#7777=EDGE_CURVE('',#6303,#6305,#3662,.T.);
#7778=EDGE_CURVE('',#6306,#6304,#3663,.T.);
#7779=EDGE_CURVE('',#6305,#6306,#3664,.T.);
#7780=EDGE_CURVE('',#6305,#6307,#3665,.T.);
#7781=EDGE_CURVE('',#6308,#6306,#3666,.T.);
#7782=EDGE_CURVE('',#6307,#6308,#3667,.T.);
#7783=EDGE_CURVE('',#6307,#6309,#3668,.T.);
#7784=EDGE_CURVE('',#6310,#6308,#3669,.T.);
#7785=EDGE_CURVE('',#6309,#6310,#3670,.T.);
#7786=EDGE_CURVE('',#6309,#6311,#3671,.T.);
#7787=EDGE_CURVE('',#6312,#6310,#3672,.T.);
#7788=EDGE_CURVE('',#6311,#6312,#3673,.T.);
#7789=EDGE_CURVE('',#6311,#6313,#3674,.T.);
#7790=EDGE_CURVE('',#6314,#6312,#3675,.T.);
#7791=EDGE_CURVE('',#6313,#6314,#3676,.T.);
#7792=EDGE_CURVE('',#6313,#6315,#3677,.T.);
#7793=EDGE_CURVE('',#6316,#6314,#3678,.T.);
#7794=EDGE_CURVE('',#6315,#6316,#3679,.T.);
#7795=EDGE_CURVE('',#6315,#6317,#3680,.T.);
#7796=EDGE_CURVE('',#6318,#6316,#3681,.T.);
#7797=EDGE_CURVE('',#6317,#6318,#3682,.T.);
#7798=EDGE_CURVE('',#6317,#6319,#3683,.T.);
#7799=EDGE_CURVE('',#6320,#6318,#3684,.T.);
#7800=EDGE_CURVE('',#6319,#6320,#3685,.T.);
#7801=EDGE_CURVE('',#6319,#6321,#3686,.T.);
#7802=EDGE_CURVE('',#6322,#6320,#3687,.T.);
#7803=EDGE_CURVE('',#6321,#6322,#3688,.T.);
#7804=EDGE_CURVE('',#6321,#5998,#3689,.T.);
#7805=EDGE_CURVE('',#5999,#6322,#3690,.T.);
#7806=EDGE_CURVE('',#6323,#6323,#5426,.T.);
#7807=EDGE_CURVE('',#6323,#6000,#3691,.T.);
#7808=EDGE_CURVE('',#5997,#6324,#3692,.T.);
#7809=EDGE_CURVE('',#6324,#6324,#5427,.T.);
#7810=EDGE_CURVE('',#6325,#6325,#5428,.T.);
#7811=EDGE_CURVE('',#6325,#6326,#3693,.T.);
#7812=EDGE_CURVE('',#6326,#6326,#5429,.T.);
#7813=EDGE_CURVE('',#6327,#6327,#5430,.T.);
#7814=EDGE_CURVE('',#6327,#6328,#3694,.T.);
#7815=EDGE_CURVE('',#6328,#6328,#5431,.T.);
#7816=EDGE_CURVE('',#6329,#6330,#453,.T.);
#7817=EDGE_CURVE('',#6330,#6329,#454,.T.);
#7818=EDGE_CURVE('',#6330,#6331,#3695,.T.);
#7819=EDGE_CURVE('',#6332,#6331,#455,.T.);
#7820=EDGE_CURVE('',#6331,#6332,#456,.T.);
#7821=EDGE_CURVE('',#6333,#6334,#3696,.T.);
#7822=EDGE_CURVE('',#6333,#6335,#3697,.T.);
#7823=EDGE_CURVE('',#6336,#6335,#3698,.T.);
#7824=EDGE_CURVE('',#6334,#6336,#3699,.T.);
#7825=EDGE_CURVE('',#6337,#6338,#3700,.T.);
#7826=EDGE_CURVE('',#6337,#6339,#3701,.T.);
#7827=EDGE_CURVE('',#6340,#6339,#3702,.T.);
#7828=EDGE_CURVE('',#6338,#6340,#3703,.T.);
#7829=EDGE_CURVE('',#6341,#6333,#3704,.T.);
#7830=EDGE_CURVE('',#6342,#6341,#3705,.T.);
#7831=EDGE_CURVE('',#6335,#6342,#3706,.T.);
#7832=EDGE_CURVE('',#6343,#6337,#3707,.T.);
#7833=EDGE_CURVE('',#6344,#6343,#3708,.T.);
#7834=EDGE_CURVE('',#6339,#6344,#3709,.T.);
#7835=EDGE_CURVE('',#6342,#6340,#5432,.T.);
#7836=EDGE_CURVE('',#6344,#6336,#5433,.T.);
#7837=EDGE_CURVE('',#6343,#6334,#5434,.T.);
#7838=EDGE_CURVE('',#6341,#6338,#5435,.T.);
#7839=EDGE_CURVE('',#6345,#6346,#3710,.T.);
#7840=EDGE_CURVE('',#6345,#6347,#3711,.T.);
#7841=EDGE_CURVE('',#6347,#6348,#3712,.T.);
#7842=EDGE_CURVE('',#6346,#6348,#3713,.T.);
#7843=EDGE_CURVE('',#6349,#6345,#3714,.T.);
#7844=EDGE_CURVE('',#6349,#6350,#3715,.T.);
#7845=EDGE_CURVE('',#6350,#6347,#3716,.T.);
#7846=EDGE_CURVE('',#6351,#6349,#3717,.T.);
#7847=EDGE_CURVE('',#6351,#6352,#3718,.T.);
#7848=EDGE_CURVE('',#6352,#6350,#3719,.T.);
#7849=EDGE_CURVE('',#6353,#6351,#3720,.T.);
#7850=EDGE_CURVE('',#6353,#6354,#3721,.T.);
#7851=EDGE_CURVE('',#6354,#6352,#3722,.T.);
#7852=EDGE_CURVE('',#6355,#6353,#3723,.T.);
#7853=EDGE_CURVE('',#6355,#6356,#3724,.T.);
#7854=EDGE_CURVE('',#6356,#6354,#3725,.T.);
#7855=EDGE_CURVE('',#6346,#6355,#3726,.T.);
#7856=EDGE_CURVE('',#6348,#6356,#3727,.T.);
#7857=EDGE_CURVE('',#6357,#6357,#5436,.T.);
#7858=EDGE_CURVE('',#6358,#6358,#5437,.T.);
#7859=EDGE_CURVE('',#6358,#6357,#3728,.T.);
#7860=EDGE_CURVE('',#6359,#6359,#5438,.F.);
#7861=EDGE_CURVE('',#6359,#6358,#3729,.T.);
#7862=EDGE_CURVE('',#6360,#6360,#5439,.T.);
#7863=EDGE_CURVE('',#6360,#6359,#3730,.T.);
#7864=EDGE_CURVE('',#6361,#6361,#5440,.T.);
#7865=EDGE_CURVE('',#6361,#6362,#3731,.T.);
#7866=EDGE_CURVE('',#6362,#6362,#5441,.T.);
#7867=EDGE_CURVE('',#6363,#6363,#5442,.T.);
#7868=EDGE_CURVE('',#6363,#6364,#3732,.T.);
#7869=EDGE_CURVE('',#6364,#6364,#5443,.T.);
#7870=EDGE_CURVE('',#6365,#6366,#3733,.T.);
#7871=EDGE_CURVE('',#6365,#6367,#3734,.T.);
#7872=EDGE_CURVE('',#6368,#6367,#3735,.T.);
#7873=EDGE_CURVE('',#6368,#6366,#3736,.T.);
#7874=EDGE_CURVE('',#6366,#6369,#5444,.T.);
#7875=EDGE_CURVE('',#6370,#6368,#3737,.T.);
#7876=EDGE_CURVE('',#6369,#6370,#3738,.T.);
#7877=EDGE_CURVE('',#6367,#6371,#3739,.T.);
#7878=EDGE_CURVE('',#6370,#6371,#3740,.T.);
#7879=EDGE_CURVE('',#6369,#6372,#3741,.T.);
#7880=EDGE_CURVE('',#6371,#6372,#3742,.T.);
#7881=EDGE_CURVE('',#6372,#6365,#5445,.T.);
#7882=EDGE_CURVE('',#6373,#6374,#3743,.T.);
#7883=EDGE_CURVE('',#6373,#6375,#3744,.T.);
#7884=EDGE_CURVE('',#6376,#6375,#3745,.T.);
#7885=EDGE_CURVE('',#6376,#6374,#3746,.T.);
#7886=EDGE_CURVE('',#6374,#6377,#5446,.T.);
#7887=EDGE_CURVE('',#6378,#6376,#3747,.T.);
#7888=EDGE_CURVE('',#6377,#6378,#3748,.T.);
#7889=EDGE_CURVE('',#6375,#6379,#3749,.T.);
#7890=EDGE_CURVE('',#6378,#6379,#3750,.T.);
#7891=EDGE_CURVE('',#6377,#6380,#3751,.T.);
#7892=EDGE_CURVE('',#6379,#6380,#3752,.T.);
#7893=EDGE_CURVE('',#6380,#6373,#5447,.T.);
#7894=EDGE_CURVE('',#6381,#6381,#5448,.T.);
#7895=EDGE_CURVE('',#6381,#6382,#3753,.T.);
#7896=EDGE_CURVE('',#6382,#6382,#5449,.T.);
#7897=EDGE_CURVE('',#6383,#6383,#5450,.T.);
#7898=EDGE_CURVE('',#6383,#6384,#3754,.T.);
#7899=EDGE_CURVE('',#6384,#6384,#5451,.T.);
#7900=EDGE_CURVE('',#6385,#6385,#5452,.T.);
#7901=EDGE_CURVE('',#6385,#6386,#3755,.T.);
#7902=EDGE_CURVE('',#6386,#6386,#5453,.T.);
#7903=EDGE_CURVE('',#6387,#6387,#5454,.T.);
#7904=EDGE_CURVE('',#6387,#6388,#3756,.T.);
#7905=EDGE_CURVE('',#6388,#6388,#5455,.T.);
#7906=EDGE_CURVE('',#6389,#6389,#5456,.T.);
#7907=EDGE_CURVE('',#6389,#6390,#3757,.T.);
#7908=EDGE_CURVE('',#6390,#6390,#5457,.T.);
#7909=EDGE_CURVE('',#6391,#6391,#5458,.T.);
#7910=EDGE_CURVE('',#6391,#6392,#3758,.T.);
#7911=EDGE_CURVE('',#6392,#6392,#5459,.T.);
#7912=EDGE_CURVE('',#6393,#6393,#5460,.T.);
#7913=EDGE_CURVE('',#6393,#6394,#3759,.T.);
#7914=EDGE_CURVE('',#6394,#6394,#5461,.T.);
#7915=EDGE_CURVE('',#6395,#6395,#5462,.T.);
#7916=EDGE_CURVE('',#6395,#6396,#3760,.T.);
#7917=EDGE_CURVE('',#6396,#6396,#5463,.T.);
#7918=EDGE_CURVE('',#6397,#6397,#5464,.T.);
#7919=EDGE_CURVE('',#6397,#6398,#3761,.T.);
#7920=EDGE_CURVE('',#6398,#6398,#5465,.T.);
#7921=EDGE_CURVE('',#6399,#6400,#3762,.T.);
#7922=EDGE_CURVE('',#6400,#6401,#3763,.T.);
#7923=EDGE_CURVE('',#6402,#6401,#3764,.T.);
#7924=EDGE_CURVE('',#6399,#6402,#3765,.T.);
#7925=EDGE_CURVE('',#6403,#6399,#3766,.T.);
#7926=EDGE_CURVE('',#6404,#6402,#3767,.T.);
#7927=EDGE_CURVE('',#6403,#6404,#3768,.T.);
#7928=EDGE_CURVE('',#6405,#6403,#3769,.T.);
#7929=EDGE_CURVE('',#6406,#6404,#3770,.T.);
#7930=EDGE_CURVE('',#6405,#6406,#3771,.T.);
#7931=EDGE_CURVE('',#6400,#6405,#3772,.T.);
#7932=EDGE_CURVE('',#6401,#6406,#3773,.T.);
#7933=EDGE_CURVE('',#6407,#6408,#3774,.T.);
#7934=EDGE_CURVE('',#6408,#6409,#3775,.T.);
#7935=EDGE_CURVE('',#6410,#6409,#3776,.T.);
#7936=EDGE_CURVE('',#6407,#6410,#3777,.T.);
#7937=EDGE_CURVE('',#6411,#6407,#3778,.T.);
#7938=EDGE_CURVE('',#6412,#6410,#3779,.T.);
#7939=EDGE_CURVE('',#6411,#6412,#3780,.T.);
#7940=EDGE_CURVE('',#6413,#6411,#3781,.T.);
#7941=EDGE_CURVE('',#6414,#6412,#3782,.T.);
#7942=EDGE_CURVE('',#6413,#6414,#3783,.T.);
#7943=EDGE_CURVE('',#6408,#6413,#3784,.T.);
#7944=EDGE_CURVE('',#6409,#6414,#3785,.T.);
#7945=EDGE_CURVE('',#6415,#6415,#5466,.T.);
#7946=EDGE_CURVE('',#6415,#6416,#3786,.T.);
#7947=EDGE_CURVE('',#6416,#6416,#5467,.T.);
#7948=EDGE_CURVE('',#6417,#6418,#3787,.T.);
#7949=EDGE_CURVE('',#6417,#6419,#3788,.T.);
#7950=EDGE_CURVE('',#6420,#6419,#3789,.T.);
#7951=EDGE_CURVE('',#6418,#6420,#3790,.T.);
#7952=EDGE_CURVE('',#6421,#6417,#3791,.T.);
#7953=EDGE_CURVE('',#6421,#6422,#3792,.T.);
#7954=EDGE_CURVE('',#6419,#6422,#3793,.T.);
#7955=EDGE_CURVE('',#6423,#6421,#3794,.T.);
#7956=EDGE_CURVE('',#6424,#6423,#3795,.T.);
#7957=EDGE_CURVE('',#6422,#6424,#3796,.T.);
#7958=EDGE_CURVE('',#6425,#6425,#5468,.T.);
#7959=EDGE_CURVE('',#6424,#6420,#5469,.T.);
#7960=EDGE_CURVE('',#6423,#6418,#5470,.T.);
#7961=EDGE_CURVE('',#6426,#6427,#3797,.T.);
#7962=EDGE_CURVE('',#6428,#6426,#5471,.T.);
#7963=EDGE_CURVE('',#6429,#6428,#3798,.T.);
#7964=EDGE_CURVE('',#6429,#6427,#5472,.T.);
#7965=EDGE_CURVE('',#6430,#6427,#3799,.T.);
#7966=EDGE_CURVE('',#6431,#6430,#3800,.T.);
#7967=EDGE_CURVE('',#6426,#6431,#3801,.T.);
#7968=EDGE_CURVE('',#6429,#6432,#3802,.T.);
#7969=EDGE_CURVE('',#6430,#6432,#5473,.T.);
#7970=EDGE_CURVE('',#6433,#6428,#3803,.T.);
#7971=EDGE_CURVE('',#6432,#6433,#3804,.T.);
#7972=EDGE_CURVE('',#6433,#6431,#5474,.T.);
#7973=EDGE_CURVE('',#6425,#6434,#3805,.T.);
#7974=EDGE_CURVE('',#6434,#6434,#5475,.T.);
#7975=EDGE_CURVE('',#6435,#6435,#5476,.T.);
#7976=EDGE_CURVE('',#6435,#6436,#3806,.T.);
#7977=EDGE_CURVE('',#6436,#6436,#5477,.T.);
#7978=EDGE_CURVE('',#6437,#6437,#5478,.T.);
#7979=EDGE_CURVE('',#6437,#6438,#3807,.T.);
#7980=EDGE_CURVE('',#6438,#6438,#5479,.T.);
#7981=EDGE_CURVE('',#6439,#6439,#5480,.T.);
#7982=EDGE_CURVE('',#6439,#6440,#3808,.T.);
#7983=EDGE_CURVE('',#6440,#6440,#5481,.T.);
#7984=EDGE_CURVE('',#6441,#6441,#5482,.T.);
#7985=EDGE_CURVE('',#6441,#6442,#3809,.T.);
#7986=EDGE_CURVE('',#6442,#6442,#5483,.T.);
#7987=EDGE_CURVE('',#6443,#6443,#5484,.T.);
#7988=EDGE_CURVE('',#6443,#6444,#3810,.T.);
#7989=EDGE_CURVE('',#6444,#6444,#5485,.T.);
#7990=EDGE_CURVE('',#6445,#6445,#5486,.T.);
#7991=EDGE_CURVE('',#6445,#6446,#3811,.T.);
#7992=EDGE_CURVE('',#6446,#6446,#5487,.T.);
#7993=EDGE_CURVE('',#6447,#6448,#3812,.T.);
#7994=EDGE_CURVE('',#6449,#6447,#3813,.T.);
#7995=EDGE_CURVE('',#6450,#6449,#3814,.T.);
#7996=EDGE_CURVE('',#6448,#6450,#3815,.T.);
#7997=EDGE_CURVE('',#6451,#6447,#3816,.T.);
#7998=EDGE_CURVE('',#6451,#6452,#3817,.T.);
#7999=EDGE_CURVE('',#6449,#6452,#3818,.T.);
#8000=EDGE_CURVE('',#6453,#6451,#3819,.T.);
#8001=EDGE_CURVE('',#6454,#6453,#3820,.T.);
#8002=EDGE_CURVE('',#6452,#6454,#3821,.T.);
#8003=EDGE_CURVE('',#6455,#6456,#5488,.T.);
#8004=EDGE_CURVE('',#6456,#6457,#51,.T.);
#8005=EDGE_CURVE('',#6457,#6458,#3822,.T.);
#8006=EDGE_CURVE('',#6458,#6459,#52,.T.);
#8007=EDGE_CURVE('',#6459,#6460,#5489,.T.);
#8008=EDGE_CURVE('',#6460,#6461,#53,.T.);
#8009=EDGE_CURVE('',#6461,#6462,#3823,.T.);
#8010=EDGE_CURVE('',#6462,#6463,#54,.T.);
#8011=EDGE_CURVE('',#6463,#6464,#5490,.T.);
#8012=EDGE_CURVE('',#6464,#6465,#55,.T.);
#8013=EDGE_CURVE('',#6465,#6466,#3824,.T.);
#8014=EDGE_CURVE('',#6466,#6467,#56,.T.);
#8015=EDGE_CURVE('',#6467,#6468,#5491,.T.);
#8016=EDGE_CURVE('',#6468,#6469,#57,.T.);
#8017=EDGE_CURVE('',#6469,#6470,#3825,.T.);
#8018=EDGE_CURVE('',#6470,#6471,#58,.T.);
#8019=EDGE_CURVE('',#6471,#6472,#5492,.T.);
#8020=EDGE_CURVE('',#6472,#6473,#59,.T.);
#8021=EDGE_CURVE('',#6473,#6474,#3826,.T.);
#8022=EDGE_CURVE('',#6474,#6475,#60,.T.);
#8023=EDGE_CURVE('',#6475,#6476,#5493,.T.);
#8024=EDGE_CURVE('',#6476,#6477,#61,.T.);
#8025=EDGE_CURVE('',#6477,#6478,#3827,.T.);
#8026=EDGE_CURVE('',#6478,#6479,#62,.T.);
#8027=EDGE_CURVE('',#6479,#6480,#5494,.T.);
#8028=EDGE_CURVE('',#6480,#6481,#63,.T.);
#8029=EDGE_CURVE('',#6481,#6482,#3828,.T.);
#8030=EDGE_CURVE('',#6482,#6483,#64,.T.);
#8031=EDGE_CURVE('',#6483,#6484,#5495,.T.);
#8032=EDGE_CURVE('',#6484,#6485,#65,.T.);
#8033=EDGE_CURVE('',#6485,#6486,#3829,.T.);
#8034=EDGE_CURVE('',#6486,#6487,#66,.T.);
#8035=EDGE_CURVE('',#6487,#6488,#5496,.T.);
#8036=EDGE_CURVE('',#6488,#6489,#67,.T.);
#8037=EDGE_CURVE('',#6489,#6490,#3830,.T.);
#8038=EDGE_CURVE('',#6490,#6491,#68,.T.);
#8039=EDGE_CURVE('',#6491,#6492,#5497,.T.);
#8040=EDGE_CURVE('',#6492,#6493,#69,.T.);
#8041=EDGE_CURVE('',#6493,#6494,#3831,.T.);
#8042=EDGE_CURVE('',#6494,#6495,#70,.T.);
#8043=EDGE_CURVE('',#6495,#6496,#5498,.T.);
#8044=EDGE_CURVE('',#6496,#6497,#71,.T.);
#8045=EDGE_CURVE('',#6497,#6498,#3832,.T.);
#8046=EDGE_CURVE('',#6498,#6499,#72,.T.);
#8047=EDGE_CURVE('',#6499,#6500,#5499,.T.);
#8048=EDGE_CURVE('',#6500,#6501,#73,.T.);
#8049=EDGE_CURVE('',#6501,#6502,#3833,.T.);
#8050=EDGE_CURVE('',#6502,#6503,#74,.T.);
#8051=EDGE_CURVE('',#6503,#6504,#5500,.T.);
#8052=EDGE_CURVE('',#6504,#6505,#75,.T.);
#8053=EDGE_CURVE('',#6505,#6506,#3834,.T.);
#8054=EDGE_CURVE('',#6506,#6507,#76,.T.);
#8055=EDGE_CURVE('',#6507,#6508,#5501,.T.);
#8056=EDGE_CURVE('',#6508,#6509,#77,.T.);
#8057=EDGE_CURVE('',#6509,#6510,#3835,.T.);
#8058=EDGE_CURVE('',#6510,#6511,#78,.T.);
#8059=EDGE_CURVE('',#6511,#6512,#5502,.T.);
#8060=EDGE_CURVE('',#6512,#6513,#79,.T.);
#8061=EDGE_CURVE('',#6513,#6514,#3836,.T.);
#8062=EDGE_CURVE('',#6514,#6515,#80,.T.);
#8063=EDGE_CURVE('',#6515,#6516,#5503,.T.);
#8064=EDGE_CURVE('',#6516,#6517,#81,.T.);
#8065=EDGE_CURVE('',#6517,#6518,#3837,.T.);
#8066=EDGE_CURVE('',#6518,#6519,#82,.T.);
#8067=EDGE_CURVE('',#6519,#6520,#5504,.T.);
#8068=EDGE_CURVE('',#6520,#6521,#83,.T.);
#8069=EDGE_CURVE('',#6521,#6522,#3838,.T.);
#8070=EDGE_CURVE('',#6522,#6523,#84,.T.);
#8071=EDGE_CURVE('',#6523,#6524,#5505,.T.);
#8072=EDGE_CURVE('',#6524,#6525,#85,.T.);
#8073=EDGE_CURVE('',#6525,#6526,#3839,.T.);
#8074=EDGE_CURVE('',#6526,#6527,#86,.T.);
#8075=EDGE_CURVE('',#6527,#6528,#5506,.T.);
#8076=EDGE_CURVE('',#6528,#6529,#87,.T.);
#8077=EDGE_CURVE('',#6529,#6530,#3840,.T.);
#8078=EDGE_CURVE('',#6530,#6531,#88,.T.);
#8079=EDGE_CURVE('',#6531,#6532,#5507,.T.);
#8080=EDGE_CURVE('',#6532,#6533,#89,.T.);
#8081=EDGE_CURVE('',#6533,#6534,#3841,.T.);
#8082=EDGE_CURVE('',#6534,#6455,#90,.T.);
#8083=EDGE_CURVE('',#6454,#6450,#5508,.T.);
#8084=EDGE_CURVE('',#6448,#6453,#5509,.T.);
#8085=EDGE_CURVE('',#6535,#6535,#5510,.T.);
#8086=EDGE_CURVE('',#6535,#6536,#3842,.T.);
#8087=EDGE_CURVE('',#6536,#6536,#5511,.T.);
#8088=EDGE_CURVE('',#6537,#6532,#3843,.T.);
#8089=EDGE_CURVE('',#6538,#6537,#91,.T.);
#8090=EDGE_CURVE('',#6533,#6538,#3844,.T.);
#8091=EDGE_CURVE('',#6539,#6538,#3845,.T.);
#8092=EDGE_CURVE('',#6534,#6539,#3846,.T.);
#8093=EDGE_CURVE('',#6540,#6539,#92,.T.);
#8094=EDGE_CURVE('',#6455,#6540,#3847,.T.);
#8095=EDGE_CURVE('',#6541,#6540,#5512,.T.);
#8096=EDGE_CURVE('',#6541,#6456,#3848,.T.);
#8097=EDGE_CURVE('',#6542,#6541,#93,.T.);
#8098=EDGE_CURVE('',#6457,#6542,#3849,.T.);
#8099=EDGE_CURVE('',#6543,#6542,#3850,.T.);
#8100=EDGE_CURVE('',#6458,#6543,#3851,.T.);
#8101=EDGE_CURVE('',#6544,#6543,#94,.T.);
#8102=EDGE_CURVE('',#6459,#6544,#3852,.T.);
#8103=EDGE_CURVE('',#6545,#6544,#5513,.T.);
#8104=EDGE_CURVE('',#6545,#6460,#3853,.T.);
#8105=EDGE_CURVE('',#6546,#6545,#95,.T.);
#8106=EDGE_CURVE('',#6461,#6546,#3854,.T.);
#8107=EDGE_CURVE('',#6547,#6546,#3855,.T.);
#8108=EDGE_CURVE('',#6462,#6547,#3856,.T.);
#8109=EDGE_CURVE('',#6548,#6547,#96,.T.);
#8110=EDGE_CURVE('',#6463,#6548,#3857,.T.);
#8111=EDGE_CURVE('',#6549,#6548,#5514,.T.);
#8112=EDGE_CURVE('',#6549,#6464,#3858,.T.);
#8113=EDGE_CURVE('',#6550,#6549,#97,.T.);
#8114=EDGE_CURVE('',#6465,#6550,#3859,.T.);
#8115=EDGE_CURVE('',#6551,#6550,#3860,.T.);
#8116=EDGE_CURVE('',#6466,#6551,#3861,.T.);
#8117=EDGE_CURVE('',#6552,#6551,#98,.T.);
#8118=EDGE_CURVE('',#6467,#6552,#3862,.T.);
#8119=EDGE_CURVE('',#6553,#6552,#5515,.T.);
#8120=EDGE_CURVE('',#6553,#6468,#3863,.T.);
#8121=EDGE_CURVE('',#6554,#6553,#99,.T.);
#8122=EDGE_CURVE('',#6469,#6554,#3864,.T.);
#8123=EDGE_CURVE('',#6555,#6554,#3865,.T.);
#8124=EDGE_CURVE('',#6470,#6555,#3866,.T.);
#8125=EDGE_CURVE('',#6556,#6555,#100,.T.);
#8126=EDGE_CURVE('',#6471,#6556,#3867,.T.);
#8127=EDGE_CURVE('',#6557,#6556,#5516,.T.);
#8128=EDGE_CURVE('',#6557,#6472,#3868,.T.);
#8129=EDGE_CURVE('',#6558,#6557,#101,.T.);
#8130=EDGE_CURVE('',#6473,#6558,#3869,.T.);
#8131=EDGE_CURVE('',#6559,#6558,#3870,.T.);
#8132=EDGE_CURVE('',#6474,#6559,#3871,.T.);
#8133=EDGE_CURVE('',#6560,#6559,#102,.T.);
#8134=EDGE_CURVE('',#6475,#6560,#3872,.T.);
#8135=EDGE_CURVE('',#6561,#6560,#5517,.T.);
#8136=EDGE_CURVE('',#6561,#6476,#3873,.T.);
#8137=EDGE_CURVE('',#6562,#6561,#103,.T.);
#8138=EDGE_CURVE('',#6477,#6562,#3874,.T.);
#8139=EDGE_CURVE('',#6563,#6562,#3875,.T.);
#8140=EDGE_CURVE('',#6478,#6563,#3876,.T.);
#8141=EDGE_CURVE('',#6564,#6563,#104,.T.);
#8142=EDGE_CURVE('',#6479,#6564,#3877,.T.);
#8143=EDGE_CURVE('',#6565,#6564,#5518,.T.);
#8144=EDGE_CURVE('',#6565,#6480,#3878,.T.);
#8145=EDGE_CURVE('',#6566,#6565,#105,.T.);
#8146=EDGE_CURVE('',#6481,#6566,#3879,.T.);
#8147=EDGE_CURVE('',#6567,#6566,#3880,.T.);
#8148=EDGE_CURVE('',#6482,#6567,#3881,.T.);
#8149=EDGE_CURVE('',#6568,#6567,#106,.T.);
#8150=EDGE_CURVE('',#6483,#6568,#3882,.T.);
#8151=EDGE_CURVE('',#6569,#6568,#5519,.T.);
#8152=EDGE_CURVE('',#6569,#6484,#3883,.T.);
#8153=EDGE_CURVE('',#6570,#6569,#107,.T.);
#8154=EDGE_CURVE('',#6485,#6570,#3884,.T.);
#8155=EDGE_CURVE('',#6571,#6570,#3885,.T.);
#8156=EDGE_CURVE('',#6486,#6571,#3886,.T.);
#8157=EDGE_CURVE('',#6572,#6571,#108,.T.);
#8158=EDGE_CURVE('',#6487,#6572,#3887,.T.);
#8159=EDGE_CURVE('',#6573,#6572,#5520,.T.);
#8160=EDGE_CURVE('',#6573,#6488,#3888,.T.);
#8161=EDGE_CURVE('',#6574,#6573,#109,.T.);
#8162=EDGE_CURVE('',#6489,#6574,#3889,.T.);
#8163=EDGE_CURVE('',#6575,#6574,#3890,.T.);
#8164=EDGE_CURVE('',#6490,#6575,#3891,.T.);
#8165=EDGE_CURVE('',#6576,#6575,#110,.T.);
#8166=EDGE_CURVE('',#6491,#6576,#3892,.T.);
#8167=EDGE_CURVE('',#6577,#6576,#5521,.T.);
#8168=EDGE_CURVE('',#6577,#6492,#3893,.T.);
#8169=EDGE_CURVE('',#6578,#6577,#111,.T.);
#8170=EDGE_CURVE('',#6493,#6578,#3894,.T.);
#8171=EDGE_CURVE('',#6579,#6578,#3895,.T.);
#8172=EDGE_CURVE('',#6494,#6579,#3896,.T.);
#8173=EDGE_CURVE('',#6580,#6579,#112,.T.);
#8174=EDGE_CURVE('',#6495,#6580,#3897,.T.);
#8175=EDGE_CURVE('',#6581,#6580,#5522,.T.);
#8176=EDGE_CURVE('',#6581,#6496,#3898,.T.);
#8177=EDGE_CURVE('',#6582,#6581,#113,.T.);
#8178=EDGE_CURVE('',#6497,#6582,#3899,.T.);
#8179=EDGE_CURVE('',#6583,#6582,#3900,.T.);
#8180=EDGE_CURVE('',#6498,#6583,#3901,.T.);
#8181=EDGE_CURVE('',#6584,#6583,#114,.T.);
#8182=EDGE_CURVE('',#6499,#6584,#3902,.T.);
#8183=EDGE_CURVE('',#6585,#6584,#5523,.T.);
#8184=EDGE_CURVE('',#6585,#6500,#3903,.T.);
#8185=EDGE_CURVE('',#6586,#6585,#115,.T.);
#8186=EDGE_CURVE('',#6501,#6586,#3904,.T.);
#8187=EDGE_CURVE('',#6587,#6586,#3905,.T.);
#8188=EDGE_CURVE('',#6502,#6587,#3906,.T.);
#8189=EDGE_CURVE('',#6588,#6587,#116,.T.);
#8190=EDGE_CURVE('',#6503,#6588,#3907,.T.);
#8191=EDGE_CURVE('',#6589,#6588,#5524,.T.);
#8192=EDGE_CURVE('',#6589,#6504,#3908,.T.);
#8193=EDGE_CURVE('',#6590,#6589,#117,.T.);
#8194=EDGE_CURVE('',#6505,#6590,#3909,.T.);
#8195=EDGE_CURVE('',#6591,#6590,#3910,.T.);
#8196=EDGE_CURVE('',#6506,#6591,#3911,.T.);
#8197=EDGE_CURVE('',#6592,#6591,#118,.T.);
#8198=EDGE_CURVE('',#6507,#6592,#3912,.T.);
#8199=EDGE_CURVE('',#6593,#6592,#5525,.T.);
#8200=EDGE_CURVE('',#6593,#6508,#3913,.T.);
#8201=EDGE_CURVE('',#6594,#6593,#119,.T.);
#8202=EDGE_CURVE('',#6509,#6594,#3914,.T.);
#8203=EDGE_CURVE('',#6595,#6594,#3915,.T.);
#8204=EDGE_CURVE('',#6510,#6595,#3916,.T.);
#8205=EDGE_CURVE('',#6596,#6595,#120,.T.);
#8206=EDGE_CURVE('',#6511,#6596,#3917,.T.);
#8207=EDGE_CURVE('',#6597,#6596,#5526,.T.);
#8208=EDGE_CURVE('',#6597,#6512,#3918,.T.);
#8209=EDGE_CURVE('',#6598,#6597,#121,.T.);
#8210=EDGE_CURVE('',#6513,#6598,#3919,.T.);
#8211=EDGE_CURVE('',#6599,#6598,#3920,.T.);
#8212=EDGE_CURVE('',#6514,#6599,#3921,.T.);
#8213=EDGE_CURVE('',#6600,#6599,#122,.T.);
#8214=EDGE_CURVE('',#6515,#6600,#3922,.T.);
#8215=EDGE_CURVE('',#6601,#6600,#5527,.T.);
#8216=EDGE_CURVE('',#6601,#6516,#3923,.T.);
#8217=EDGE_CURVE('',#6602,#6601,#123,.T.);
#8218=EDGE_CURVE('',#6517,#6602,#3924,.T.);
#8219=EDGE_CURVE('',#6603,#6602,#3925,.T.);
#8220=EDGE_CURVE('',#6518,#6603,#3926,.T.);
#8221=EDGE_CURVE('',#6604,#6603,#124,.T.);
#8222=EDGE_CURVE('',#6519,#6604,#3927,.T.);
#8223=EDGE_CURVE('',#6605,#6604,#5528,.T.);
#8224=EDGE_CURVE('',#6605,#6520,#3928,.T.);
#8225=EDGE_CURVE('',#6606,#6605,#125,.T.);
#8226=EDGE_CURVE('',#6521,#6606,#3929,.T.);
#8227=EDGE_CURVE('',#6607,#6606,#3930,.T.);
#8228=EDGE_CURVE('',#6522,#6607,#3931,.T.);
#8229=EDGE_CURVE('',#6608,#6607,#126,.T.);
#8230=EDGE_CURVE('',#6523,#6608,#3932,.T.);
#8231=EDGE_CURVE('',#6609,#6608,#5529,.T.);
#8232=EDGE_CURVE('',#6609,#6524,#3933,.T.);
#8233=EDGE_CURVE('',#6610,#6609,#127,.T.);
#8234=EDGE_CURVE('',#6525,#6610,#3934,.T.);
#8235=EDGE_CURVE('',#6611,#6610,#3935,.T.);
#8236=EDGE_CURVE('',#6526,#6611,#3936,.T.);
#8237=EDGE_CURVE('',#6612,#6611,#128,.T.);
#8238=EDGE_CURVE('',#6527,#6612,#3937,.T.);
#8239=EDGE_CURVE('',#6613,#6612,#5530,.T.);
#8240=EDGE_CURVE('',#6613,#6528,#3938,.T.);
#8241=EDGE_CURVE('',#6614,#6613,#129,.T.);
#8242=EDGE_CURVE('',#6529,#6614,#3939,.T.);
#8243=EDGE_CURVE('',#6615,#6614,#3940,.T.);
#8244=EDGE_CURVE('',#6530,#6615,#3941,.T.);
#8245=EDGE_CURVE('',#6616,#6615,#130,.T.);
#8246=EDGE_CURVE('',#6531,#6616,#3942,.T.);
#8247=EDGE_CURVE('',#6537,#6616,#5531,.T.);
#8248=EDGE_CURVE('',#6617,#6617,#5532,.T.);
#8249=EDGE_CURVE('',#6617,#6618,#3943,.T.);
#8250=EDGE_CURVE('',#6618,#6618,#5533,.T.);
#8251=EDGE_CURVE('',#6619,#6619,#5534,.T.);
#8252=EDGE_CURVE('',#6619,#6620,#3944,.T.);
#8253=EDGE_CURVE('',#6620,#6620,#5535,.T.);
#8254=EDGE_CURVE('',#6621,#6621,#5536,.T.);
#8255=EDGE_CURVE('',#6622,#6622,#5537,.T.);
#8256=EDGE_CURVE('',#6622,#6621,#3945,.T.);
#8257=EDGE_CURVE('',#6623,#6623,#5538,.T.);
#8258=EDGE_CURVE('',#6623,#6622,#3946,.T.);
#8259=EDGE_CURVE('',#6624,#6624,#5539,.T.);
#8260=EDGE_CURVE('',#6624,#6623,#3947,.T.);
#8261=EDGE_CURVE('',#6625,#6625,#5540,.T.);
#8262=EDGE_CURVE('',#6626,#6626,#5541,.F.);
#8263=EDGE_CURVE('',#6626,#6625,#3948,.T.);
#8264=EDGE_CURVE('',#6627,#6627,#5542,.F.);
#8265=EDGE_CURVE('',#6627,#6626,#3949,.T.);
#8266=EDGE_CURVE('',#6628,#6628,#5543,.T.);
#8267=EDGE_CURVE('',#6628,#6627,#3950,.T.);
#8268=EDGE_CURVE('',#6629,#6630,#3951,.T.);
#8269=EDGE_CURVE('',#6630,#6631,#3952,.T.);
#8270=EDGE_CURVE('',#6631,#6632,#3953,.T.);
#8271=EDGE_CURVE('',#6629,#6632,#3954,.T.);
#8272=EDGE_CURVE('',#6630,#6633,#3955,.T.);
#8273=EDGE_CURVE('',#6633,#6634,#3956,.T.);
#8274=EDGE_CURVE('',#6634,#6631,#3957,.T.);
#8275=EDGE_CURVE('',#6633,#6635,#3958,.T.);
#8276=EDGE_CURVE('',#6635,#6636,#3959,.T.);
#8277=EDGE_CURVE('',#6636,#6634,#3960,.T.);
#8278=EDGE_CURVE('',#6635,#6637,#3961,.T.);
#8279=EDGE_CURVE('',#6637,#6638,#3962,.T.);
#8280=EDGE_CURVE('',#6638,#6636,#3963,.T.);
#8281=EDGE_CURVE('',#6637,#6639,#3964,.T.);
#8282=EDGE_CURVE('',#6639,#6640,#3965,.T.);
#8283=EDGE_CURVE('',#6640,#6638,#3966,.T.);
#8284=EDGE_CURVE('',#6639,#6629,#3967,.T.);
#8285=EDGE_CURVE('',#6632,#6640,#3968,.T.);
#8286=EDGE_CURVE('',#6641,#6641,#5544,.T.);
#8287=EDGE_CURVE('',#6642,#6642,#5545,.T.);
#8288=EDGE_CURVE('',#6642,#6641,#3969,.T.);
#8289=EDGE_CURVE('',#6643,#6643,#5546,.T.);
#8290=EDGE_CURVE('',#6643,#6642,#3970,.T.);
#8291=EDGE_CURVE('',#6644,#6644,#5547,.T.);
#8292=EDGE_CURVE('',#6644,#6643,#3971,.T.);
#8293=EDGE_CURVE('',#6645,#6645,#5548,.T.);
#8294=EDGE_CURVE('',#6646,#6646,#5549,.F.);
#8295=EDGE_CURVE('',#6646,#6645,#3972,.T.);
#8296=EDGE_CURVE('',#6647,#6647,#5550,.F.);
#8297=EDGE_CURVE('',#6647,#6646,#3973,.T.);
#8298=EDGE_CURVE('',#6648,#6648,#5551,.T.);
#8299=EDGE_CURVE('',#6648,#6647,#3974,.T.);
#8300=EDGE_CURVE('',#6649,#6650,#3975,.T.);
#8301=EDGE_CURVE('',#6650,#6651,#3976,.T.);
#8302=EDGE_CURVE('',#6651,#6652,#3977,.T.);
#8303=EDGE_CURVE('',#6649,#6652,#3978,.T.);
#8304=EDGE_CURVE('',#6650,#6653,#3979,.T.);
#8305=EDGE_CURVE('',#6653,#6654,#3980,.T.);
#8306=EDGE_CURVE('',#6654,#6651,#3981,.T.);
#8307=EDGE_CURVE('',#6653,#6655,#3982,.T.);
#8308=EDGE_CURVE('',#6655,#6656,#3983,.T.);
#8309=EDGE_CURVE('',#6656,#6654,#3984,.T.);
#8310=EDGE_CURVE('',#6655,#6657,#3985,.T.);
#8311=EDGE_CURVE('',#6657,#6658,#3986,.T.);
#8312=EDGE_CURVE('',#6658,#6656,#3987,.T.);
#8313=EDGE_CURVE('',#6657,#6659,#3988,.T.);
#8314=EDGE_CURVE('',#6659,#6660,#3989,.T.);
#8315=EDGE_CURVE('',#6660,#6658,#3990,.T.);
#8316=EDGE_CURVE('',#6659,#6649,#3991,.T.);
#8317=EDGE_CURVE('',#6652,#6660,#3992,.T.);
#8318=EDGE_CURVE('',#6661,#6661,#5552,.T.);
#8319=EDGE_CURVE('',#6661,#6662,#3993,.T.);
#8320=EDGE_CURVE('',#6662,#6662,#5553,.T.);
#8321=EDGE_CURVE('',#6663,#6663,#5554,.T.);
#8322=EDGE_CURVE('',#6663,#6664,#3994,.T.);
#8323=EDGE_CURVE('',#6664,#6664,#5555,.T.);
#8324=ORIENTED_EDGE('',*,*,#6665,.F.);
#8325=ORIENTED_EDGE('',*,*,#6666,.T.);
#8326=ORIENTED_EDGE('',*,*,#6667,.F.);
#8327=ORIENTED_EDGE('',*,*,#6666,.F.);
#8328=ORIENTED_EDGE('',*,*,#6668,.F.);
#8329=ORIENTED_EDGE('',*,*,#6669,.T.);
#8330=ORIENTED_EDGE('',*,*,#6670,.F.);
#8331=ORIENTED_EDGE('',*,*,#6669,.F.);
#8332=ORIENTED_EDGE('',*,*,#6671,.F.);
#8333=ORIENTED_EDGE('',*,*,#6672,.T.);
#8334=ORIENTED_EDGE('',*,*,#6673,.F.);
#8335=ORIENTED_EDGE('',*,*,#6672,.F.);
#8336=ORIENTED_EDGE('',*,*,#6674,.F.);
#8337=ORIENTED_EDGE('',*,*,#6675,.T.);
#8338=ORIENTED_EDGE('',*,*,#6676,.F.);
#8339=ORIENTED_EDGE('',*,*,#6675,.F.);
#8340=ORIENTED_EDGE('',*,*,#6677,.F.);
#8341=ORIENTED_EDGE('',*,*,#6678,.T.);
#8342=ORIENTED_EDGE('',*,*,#6679,.F.);
#8343=ORIENTED_EDGE('',*,*,#6678,.F.);
#8344=ORIENTED_EDGE('',*,*,#6680,.F.);
#8345=ORIENTED_EDGE('',*,*,#6681,.T.);
#8346=ORIENTED_EDGE('',*,*,#6682,.F.);
#8347=ORIENTED_EDGE('',*,*,#6681,.F.);
#8348=ORIENTED_EDGE('',*,*,#6683,.F.);
#8349=ORIENTED_EDGE('',*,*,#6684,.T.);
#8350=ORIENTED_EDGE('',*,*,#6685,.F.);
#8351=ORIENTED_EDGE('',*,*,#6684,.F.);
#8352=ORIENTED_EDGE('',*,*,#6686,.F.);
#8353=ORIENTED_EDGE('',*,*,#6687,.T.);
#8354=ORIENTED_EDGE('',*,*,#6688,.F.);
#8355=ORIENTED_EDGE('',*,*,#6687,.F.);
#8356=ORIENTED_EDGE('',*,*,#6689,.F.);
#8357=ORIENTED_EDGE('',*,*,#6690,.T.);
#8358=ORIENTED_EDGE('',*,*,#6691,.F.);
#8359=ORIENTED_EDGE('',*,*,#6690,.F.);
#8360=ORIENTED_EDGE('',*,*,#6692,.F.);
#8361=ORIENTED_EDGE('',*,*,#6693,.T.);
#8362=ORIENTED_EDGE('',*,*,#6694,.F.);
#8363=ORIENTED_EDGE('',*,*,#6693,.F.);
#8364=ORIENTED_EDGE('',*,*,#6695,.T.);
#8365=ORIENTED_EDGE('',*,*,#6696,.T.);
#8366=ORIENTED_EDGE('',*,*,#6697,.F.);
#8367=ORIENTED_EDGE('',*,*,#6698,.F.);
#8368=ORIENTED_EDGE('',*,*,#6699,.T.);
#8369=ORIENTED_EDGE('',*,*,#6698,.T.);
#8370=ORIENTED_EDGE('',*,*,#6700,.F.);
#8371=ORIENTED_EDGE('',*,*,#6701,.F.);
#8372=ORIENTED_EDGE('',*,*,#6702,.T.);
#8373=ORIENTED_EDGE('',*,*,#6701,.T.);
#8374=ORIENTED_EDGE('',*,*,#6703,.F.);
#8375=ORIENTED_EDGE('',*,*,#6704,.F.);
#8376=ORIENTED_EDGE('',*,*,#6705,.T.);
#8377=ORIENTED_EDGE('',*,*,#6704,.T.);
#8378=ORIENTED_EDGE('',*,*,#6706,.F.);
#8379=ORIENTED_EDGE('',*,*,#6696,.F.);
#8380=ORIENTED_EDGE('',*,*,#6706,.T.);
#8381=ORIENTED_EDGE('',*,*,#6703,.T.);
#8382=ORIENTED_EDGE('',*,*,#6700,.T.);
#8383=ORIENTED_EDGE('',*,*,#6697,.T.);
#8384=ORIENTED_EDGE('',*,*,#6673,.T.);
#8385=ORIENTED_EDGE('',*,*,#6676,.T.);
#8386=ORIENTED_EDGE('',*,*,#6679,.T.);
#8387=ORIENTED_EDGE('',*,*,#6682,.T.);
#8388=ORIENTED_EDGE('',*,*,#6685,.T.);
#8389=ORIENTED_EDGE('',*,*,#6688,.T.);
#8390=ORIENTED_EDGE('',*,*,#6691,.T.);
#8391=ORIENTED_EDGE('',*,*,#6694,.T.);
#8392=ORIENTED_EDGE('',*,*,#6670,.T.);
#8393=ORIENTED_EDGE('',*,*,#6667,.T.);
#8394=ORIENTED_EDGE('',*,*,#6705,.F.);
#8395=ORIENTED_EDGE('',*,*,#6695,.F.);
#8396=ORIENTED_EDGE('',*,*,#6699,.F.);
#8397=ORIENTED_EDGE('',*,*,#6702,.F.);
#8398=ORIENTED_EDGE('',*,*,#6671,.T.);
#8399=ORIENTED_EDGE('',*,*,#6674,.T.);
#8400=ORIENTED_EDGE('',*,*,#6677,.T.);
#8401=ORIENTED_EDGE('',*,*,#6680,.T.);
#8402=ORIENTED_EDGE('',*,*,#6683,.T.);
#8403=ORIENTED_EDGE('',*,*,#6686,.T.);
#8404=ORIENTED_EDGE('',*,*,#6689,.T.);
#8405=ORIENTED_EDGE('',*,*,#6692,.T.);
#8406=ORIENTED_EDGE('',*,*,#6668,.T.);
#8407=ORIENTED_EDGE('',*,*,#6665,.T.);
#8408=ORIENTED_EDGE('',*,*,#6707,.T.);
#8409=ORIENTED_EDGE('',*,*,#6708,.T.);
#8410=ORIENTED_EDGE('',*,*,#6709,.F.);
#8411=ORIENTED_EDGE('',*,*,#6710,.F.);
#8412=ORIENTED_EDGE('',*,*,#6711,.T.);
#8413=ORIENTED_EDGE('',*,*,#6710,.T.);
#8414=ORIENTED_EDGE('',*,*,#6712,.F.);
#8415=ORIENTED_EDGE('',*,*,#6713,.F.);
#8416=ORIENTED_EDGE('',*,*,#6714,.T.);
#8417=ORIENTED_EDGE('',*,*,#6713,.T.);
#8418=ORIENTED_EDGE('',*,*,#6715,.F.);
#8419=ORIENTED_EDGE('',*,*,#6716,.F.);
#8420=ORIENTED_EDGE('',*,*,#6717,.T.);
#8421=ORIENTED_EDGE('',*,*,#6716,.T.);
#8422=ORIENTED_EDGE('',*,*,#6718,.F.);
#8423=ORIENTED_EDGE('',*,*,#6708,.F.);
#8424=ORIENTED_EDGE('',*,*,#6718,.T.);
#8425=ORIENTED_EDGE('',*,*,#6715,.T.);
#8426=ORIENTED_EDGE('',*,*,#6712,.T.);
#8427=ORIENTED_EDGE('',*,*,#6709,.T.);
#8428=ORIENTED_EDGE('',*,*,#6717,.F.);
#8429=ORIENTED_EDGE('',*,*,#6707,.F.);
#8430=ORIENTED_EDGE('',*,*,#6711,.F.);
#8431=ORIENTED_EDGE('',*,*,#6714,.F.);
#8432=ORIENTED_EDGE('',*,*,#6719,.T.);
#8433=ORIENTED_EDGE('',*,*,#6720,.T.);
#8434=ORIENTED_EDGE('',*,*,#6721,.F.);
#8435=ORIENTED_EDGE('',*,*,#6722,.F.);
#8436=ORIENTED_EDGE('',*,*,#6723,.T.);
#8437=ORIENTED_EDGE('',*,*,#6722,.T.);
#8438=ORIENTED_EDGE('',*,*,#6724,.F.);
#8439=ORIENTED_EDGE('',*,*,#6725,.F.);
#8440=ORIENTED_EDGE('',*,*,#6726,.T.);
#8441=ORIENTED_EDGE('',*,*,#6725,.T.);
#8442=ORIENTED_EDGE('',*,*,#6727,.F.);
#8443=ORIENTED_EDGE('',*,*,#6728,.F.);
#8444=ORIENTED_EDGE('',*,*,#6729,.T.);
#8445=ORIENTED_EDGE('',*,*,#6728,.T.);
#8446=ORIENTED_EDGE('',*,*,#6730,.F.);
#8447=ORIENTED_EDGE('',*,*,#6720,.F.);
#8448=ORIENTED_EDGE('',*,*,#6730,.T.);
#8449=ORIENTED_EDGE('',*,*,#6727,.T.);
#8450=ORIENTED_EDGE('',*,*,#6724,.T.);
#8451=ORIENTED_EDGE('',*,*,#6721,.T.);
#8452=ORIENTED_EDGE('',*,*,#6729,.F.);
#8453=ORIENTED_EDGE('',*,*,#6719,.F.);
#8454=ORIENTED_EDGE('',*,*,#6723,.F.);
#8455=ORIENTED_EDGE('',*,*,#6726,.F.);
#8456=ORIENTED_EDGE('',*,*,#6731,.F.);
#8457=ORIENTED_EDGE('',*,*,#6732,.T.);
#8458=ORIENTED_EDGE('',*,*,#6733,.F.);
#8459=ORIENTED_EDGE('',*,*,#6732,.F.);
#8460=ORIENTED_EDGE('',*,*,#6731,.T.);
#8461=ORIENTED_EDGE('',*,*,#6734,.F.);
#8462=ORIENTED_EDGE('',*,*,#6735,.T.);
#8463=ORIENTED_EDGE('',*,*,#6736,.F.);
#8464=ORIENTED_EDGE('',*,*,#6735,.F.);
#8465=ORIENTED_EDGE('',*,*,#6734,.T.);
#8466=ORIENTED_EDGE('',*,*,#6737,.F.);
#8467=ORIENTED_EDGE('',*,*,#6738,.F.);
#8468=ORIENTED_EDGE('',*,*,#6739,.F.);
#8469=ORIENTED_EDGE('',*,*,#6740,.F.);
#8470=ORIENTED_EDGE('',*,*,#6741,.F.);
#8471=ORIENTED_EDGE('',*,*,#6742,.F.);
#8472=ORIENTED_EDGE('',*,*,#6743,.F.);
#8473=ORIENTED_EDGE('',*,*,#6744,.F.);
#8474=ORIENTED_EDGE('',*,*,#6738,.T.);
#8475=ORIENTED_EDGE('',*,*,#6745,.F.);
#8476=ORIENTED_EDGE('',*,*,#6746,.F.);
#8477=ORIENTED_EDGE('',*,*,#6747,.F.);
#8478=ORIENTED_EDGE('',*,*,#6748,.F.);
#8479=ORIENTED_EDGE('',*,*,#6749,.F.);
#8480=ORIENTED_EDGE('',*,*,#6744,.T.);
#8481=ORIENTED_EDGE('',*,*,#6750,.T.);
#8482=ORIENTED_EDGE('',*,*,#6739,.T.);
#8483=ORIENTED_EDGE('',*,*,#6750,.F.);
#8484=ORIENTED_EDGE('',*,*,#6743,.T.);
#8485=ORIENTED_EDGE('',*,*,#6751,.F.);
#8486=ORIENTED_EDGE('',*,*,#6741,.T.);
#8487=ORIENTED_EDGE('',*,*,#6749,.T.);
#8488=ORIENTED_EDGE('',*,*,#6752,.T.);
#8489=ORIENTED_EDGE('',*,*,#6753,.F.);
#8490=ORIENTED_EDGE('',*,*,#6737,.T.);
#8491=ORIENTED_EDGE('',*,*,#6754,.F.);
#8492=ORIENTED_EDGE('',*,*,#6755,.F.);
#8493=ORIENTED_EDGE('',*,*,#6745,.T.);
#8494=ORIENTED_EDGE('',*,*,#6740,.T.);
#8495=ORIENTED_EDGE('',*,*,#6751,.T.);
#8496=ORIENTED_EDGE('',*,*,#6742,.T.);
#8497=ORIENTED_EDGE('',*,*,#6753,.T.);
#8498=ORIENTED_EDGE('',*,*,#6756,.T.);
#8499=ORIENTED_EDGE('',*,*,#6757,.F.);
#8500=ORIENTED_EDGE('',*,*,#6758,.T.);
#8501=ORIENTED_EDGE('',*,*,#6754,.T.);
#8502=ORIENTED_EDGE('',*,*,#6733,.T.);
#8503=ORIENTED_EDGE('',*,*,#6736,.T.);
#8504=ORIENTED_EDGE('',*,*,#6759,.F.);
#8505=ORIENTED_EDGE('',*,*,#6756,.F.);
#8506=ORIENTED_EDGE('',*,*,#6752,.F.);
#8507=ORIENTED_EDGE('',*,*,#6748,.T.);
#8508=ORIENTED_EDGE('',*,*,#6760,.F.);
#8509=ORIENTED_EDGE('',*,*,#6746,.T.);
#8510=ORIENTED_EDGE('',*,*,#6755,.T.);
#8511=ORIENTED_EDGE('',*,*,#6758,.F.);
#8512=ORIENTED_EDGE('',*,*,#6761,.F.);
#8513=ORIENTED_EDGE('',*,*,#6762,.T.);
#8514=ORIENTED_EDGE('',*,*,#6763,.F.);
#8515=ORIENTED_EDGE('',*,*,#6762,.F.);
#8516=ORIENTED_EDGE('',*,*,#6761,.T.);
#8517=ORIENTED_EDGE('',*,*,#6764,.F.);
#8518=ORIENTED_EDGE('',*,*,#6765,.T.);
#8519=ORIENTED_EDGE('',*,*,#6766,.F.);
#8520=ORIENTED_EDGE('',*,*,#6765,.F.);
#8521=ORIENTED_EDGE('',*,*,#6764,.T.);
#8522=ORIENTED_EDGE('',*,*,#6767,.F.);
#8523=ORIENTED_EDGE('',*,*,#6768,.F.);
#8524=ORIENTED_EDGE('',*,*,#6769,.F.);
#8525=ORIENTED_EDGE('',*,*,#6770,.F.);
#8526=ORIENTED_EDGE('',*,*,#6771,.F.);
#8527=ORIENTED_EDGE('',*,*,#6772,.F.);
#8528=ORIENTED_EDGE('',*,*,#6773,.F.);
#8529=ORIENTED_EDGE('',*,*,#6774,.F.);
#8530=ORIENTED_EDGE('',*,*,#6768,.T.);
#8531=ORIENTED_EDGE('',*,*,#6775,.F.);
#8532=ORIENTED_EDGE('',*,*,#6776,.F.);
#8533=ORIENTED_EDGE('',*,*,#6777,.F.);
#8534=ORIENTED_EDGE('',*,*,#6778,.F.);
#8535=ORIENTED_EDGE('',*,*,#6779,.F.);
#8536=ORIENTED_EDGE('',*,*,#6774,.T.);
#8537=ORIENTED_EDGE('',*,*,#6780,.T.);
#8538=ORIENTED_EDGE('',*,*,#6769,.T.);
#8539=ORIENTED_EDGE('',*,*,#6780,.F.);
#8540=ORIENTED_EDGE('',*,*,#6773,.T.);
#8541=ORIENTED_EDGE('',*,*,#6781,.F.);
#8542=ORIENTED_EDGE('',*,*,#6771,.T.);
#8543=ORIENTED_EDGE('',*,*,#6779,.T.);
#8544=ORIENTED_EDGE('',*,*,#6782,.T.);
#8545=ORIENTED_EDGE('',*,*,#6783,.F.);
#8546=ORIENTED_EDGE('',*,*,#6767,.T.);
#8547=ORIENTED_EDGE('',*,*,#6784,.F.);
#8548=ORIENTED_EDGE('',*,*,#6785,.F.);
#8549=ORIENTED_EDGE('',*,*,#6775,.T.);
#8550=ORIENTED_EDGE('',*,*,#6770,.T.);
#8551=ORIENTED_EDGE('',*,*,#6781,.T.);
#8552=ORIENTED_EDGE('',*,*,#6772,.T.);
#8553=ORIENTED_EDGE('',*,*,#6783,.T.);
#8554=ORIENTED_EDGE('',*,*,#6786,.T.);
#8555=ORIENTED_EDGE('',*,*,#6787,.F.);
#8556=ORIENTED_EDGE('',*,*,#6788,.T.);
#8557=ORIENTED_EDGE('',*,*,#6784,.T.);
#8558=ORIENTED_EDGE('',*,*,#6763,.T.);
#8559=ORIENTED_EDGE('',*,*,#6766,.T.);
#8560=ORIENTED_EDGE('',*,*,#6789,.F.);
#8561=ORIENTED_EDGE('',*,*,#6786,.F.);
#8562=ORIENTED_EDGE('',*,*,#6782,.F.);
#8563=ORIENTED_EDGE('',*,*,#6778,.T.);
#8564=ORIENTED_EDGE('',*,*,#6790,.F.);
#8565=ORIENTED_EDGE('',*,*,#6776,.T.);
#8566=ORIENTED_EDGE('',*,*,#6785,.T.);
#8567=ORIENTED_EDGE('',*,*,#6788,.F.);
#8568=ORIENTED_EDGE('',*,*,#6791,.F.);
#8569=ORIENTED_EDGE('',*,*,#6792,.T.);
#8570=ORIENTED_EDGE('',*,*,#6793,.F.);
#8571=ORIENTED_EDGE('',*,*,#6792,.F.);
#8572=ORIENTED_EDGE('',*,*,#6794,.F.);
#8573=ORIENTED_EDGE('',*,*,#6795,.T.);
#8574=ORIENTED_EDGE('',*,*,#6796,.F.);
#8575=ORIENTED_EDGE('',*,*,#6795,.F.);
#8576=ORIENTED_EDGE('',*,*,#6797,.F.);
#8577=ORIENTED_EDGE('',*,*,#6798,.T.);
#8578=ORIENTED_EDGE('',*,*,#6799,.F.);
#8579=ORIENTED_EDGE('',*,*,#6798,.F.);
#8580=ORIENTED_EDGE('',*,*,#6800,.F.);
#8581=ORIENTED_EDGE('',*,*,#6801,.T.);
#8582=ORIENTED_EDGE('',*,*,#6802,.F.);
#8583=ORIENTED_EDGE('',*,*,#6801,.F.);
#8584=ORIENTED_EDGE('',*,*,#6803,.T.);
#8585=ORIENTED_EDGE('',*,*,#6804,.T.);
#8586=ORIENTED_EDGE('',*,*,#6805,.T.);
#8587=ORIENTED_EDGE('',*,*,#6806,.T.);
#8588=ORIENTED_EDGE('',*,*,#6807,.F.);
#8589=ORIENTED_EDGE('',*,*,#6808,.F.);
#8590=ORIENTED_EDGE('',*,*,#6809,.F.);
#8591=ORIENTED_EDGE('',*,*,#6810,.F.);
#8592=ORIENTED_EDGE('',*,*,#6802,.T.);
#8593=ORIENTED_EDGE('',*,*,#6799,.T.);
#8594=ORIENTED_EDGE('',*,*,#6796,.T.);
#8595=ORIENTED_EDGE('',*,*,#6793,.T.);
#8596=ORIENTED_EDGE('',*,*,#6811,.T.);
#8597=ORIENTED_EDGE('',*,*,#6812,.T.);
#8598=ORIENTED_EDGE('',*,*,#6806,.F.);
#8599=ORIENTED_EDGE('',*,*,#6813,.F.);
#8600=ORIENTED_EDGE('',*,*,#6814,.T.);
#8601=ORIENTED_EDGE('',*,*,#6813,.T.);
#8602=ORIENTED_EDGE('',*,*,#6805,.F.);
#8603=ORIENTED_EDGE('',*,*,#6815,.F.);
#8604=ORIENTED_EDGE('',*,*,#6816,.T.);
#8605=ORIENTED_EDGE('',*,*,#6815,.T.);
#8606=ORIENTED_EDGE('',*,*,#6804,.F.);
#8607=ORIENTED_EDGE('',*,*,#6817,.F.);
#8608=ORIENTED_EDGE('',*,*,#6818,.T.);
#8609=ORIENTED_EDGE('',*,*,#6817,.T.);
#8610=ORIENTED_EDGE('',*,*,#6803,.F.);
#8611=ORIENTED_EDGE('',*,*,#6812,.F.);
#8612=ORIENTED_EDGE('',*,*,#6809,.T.);
#8613=ORIENTED_EDGE('',*,*,#6819,.T.);
#8614=ORIENTED_EDGE('',*,*,#6820,.F.);
#8615=ORIENTED_EDGE('',*,*,#6821,.F.);
#8616=ORIENTED_EDGE('',*,*,#6808,.T.);
#8617=ORIENTED_EDGE('',*,*,#6822,.T.);
#8618=ORIENTED_EDGE('',*,*,#6823,.F.);
#8619=ORIENTED_EDGE('',*,*,#6819,.F.);
#8620=ORIENTED_EDGE('',*,*,#6807,.T.);
#8621=ORIENTED_EDGE('',*,*,#6824,.T.);
#8622=ORIENTED_EDGE('',*,*,#6825,.F.);
#8623=ORIENTED_EDGE('',*,*,#6822,.F.);
#8624=ORIENTED_EDGE('',*,*,#6810,.T.);
#8625=ORIENTED_EDGE('',*,*,#6821,.T.);
#8626=ORIENTED_EDGE('',*,*,#6826,.F.);
#8627=ORIENTED_EDGE('',*,*,#6824,.F.);
#8628=ORIENTED_EDGE('',*,*,#6759,.T.);
#8629=ORIENTED_EDGE('',*,*,#6747,.T.);
#8630=ORIENTED_EDGE('',*,*,#6760,.T.);
#8631=ORIENTED_EDGE('',*,*,#6757,.T.);
#8632=ORIENTED_EDGE('',*,*,#6789,.T.);
#8633=ORIENTED_EDGE('',*,*,#6777,.T.);
#8634=ORIENTED_EDGE('',*,*,#6790,.T.);
#8635=ORIENTED_EDGE('',*,*,#6787,.T.);
#8636=ORIENTED_EDGE('',*,*,#6826,.T.);
#8637=ORIENTED_EDGE('',*,*,#6820,.T.);
#8638=ORIENTED_EDGE('',*,*,#6823,.T.);
#8639=ORIENTED_EDGE('',*,*,#6825,.T.);
#8640=ORIENTED_EDGE('',*,*,#6818,.F.);
#8641=ORIENTED_EDGE('',*,*,#6811,.F.);
#8642=ORIENTED_EDGE('',*,*,#6814,.F.);
#8643=ORIENTED_EDGE('',*,*,#6816,.F.);
#8644=ORIENTED_EDGE('',*,*,#6791,.T.);
#8645=ORIENTED_EDGE('',*,*,#6794,.T.);
#8646=ORIENTED_EDGE('',*,*,#6797,.T.);
#8647=ORIENTED_EDGE('',*,*,#6800,.T.);
#8648=ORIENTED_EDGE('',*,*,#6827,.F.);
#8649=ORIENTED_EDGE('',*,*,#6828,.T.);
#8650=ORIENTED_EDGE('',*,*,#6829,.F.);
#8651=ORIENTED_EDGE('',*,*,#6830,.F.);
#8652=ORIENTED_EDGE('',*,*,#6831,.F.);
#8653=ORIENTED_EDGE('',*,*,#6832,.F.);
#8654=ORIENTED_EDGE('',*,*,#6833,.F.);
#8655=ORIENTED_EDGE('',*,*,#6834,.F.);
#8656=ORIENTED_EDGE('',*,*,#6835,.F.);
#8657=ORIENTED_EDGE('',*,*,#6836,.F.);
#8658=ORIENTED_EDGE('',*,*,#6837,.F.);
#8659=ORIENTED_EDGE('',*,*,#6838,.F.);
#8660=ORIENTED_EDGE('',*,*,#6839,.F.);
#8661=ORIENTED_EDGE('',*,*,#6832,.T.);
#8662=ORIENTED_EDGE('',*,*,#6840,.F.);
#8663=ORIENTED_EDGE('',*,*,#6841,.F.);
#8664=ORIENTED_EDGE('',*,*,#6842,.F.);
#8665=ORIENTED_EDGE('',*,*,#6843,.F.);
#8666=ORIENTED_EDGE('',*,*,#6844,.F.);
#8667=ORIENTED_EDGE('',*,*,#6828,.F.);
#8668=ORIENTED_EDGE('',*,*,#6833,.T.);
#8669=ORIENTED_EDGE('',*,*,#6839,.T.);
#8670=ORIENTED_EDGE('',*,*,#6845,.F.);
#8671=ORIENTED_EDGE('',*,*,#6840,.T.);
#8672=ORIENTED_EDGE('',*,*,#6827,.T.);
#8673=ORIENTED_EDGE('',*,*,#6846,.F.);
#8674=ORIENTED_EDGE('',*,*,#6834,.T.);
#8675=ORIENTED_EDGE('',*,*,#6846,.T.);
#8676=ORIENTED_EDGE('',*,*,#6830,.T.);
#8677=ORIENTED_EDGE('',*,*,#6847,.F.);
#8678=ORIENTED_EDGE('',*,*,#6838,.T.);
#8679=ORIENTED_EDGE('',*,*,#6848,.F.);
#8680=ORIENTED_EDGE('',*,*,#6841,.T.);
#8681=ORIENTED_EDGE('',*,*,#6845,.T.);
#8682=ORIENTED_EDGE('',*,*,#6837,.T.);
#8683=ORIENTED_EDGE('',*,*,#6849,.F.);
#8684=ORIENTED_EDGE('',*,*,#6842,.T.);
#8685=ORIENTED_EDGE('',*,*,#6848,.T.);
#8686=ORIENTED_EDGE('',*,*,#6836,.T.);
#8687=ORIENTED_EDGE('',*,*,#6850,.F.);
#8688=ORIENTED_EDGE('',*,*,#6843,.T.);
#8689=ORIENTED_EDGE('',*,*,#6849,.T.);
#8690=ORIENTED_EDGE('',*,*,#6831,.T.);
#8691=ORIENTED_EDGE('',*,*,#6847,.T.);
#8692=ORIENTED_EDGE('',*,*,#6829,.T.);
#8693=ORIENTED_EDGE('',*,*,#6844,.T.);
#8694=ORIENTED_EDGE('',*,*,#6850,.T.);
#8695=ORIENTED_EDGE('',*,*,#6835,.T.);
#8696=ORIENTED_EDGE('',*,*,#6851,.F.);
#8697=ORIENTED_EDGE('',*,*,#6852,.T.);
#8698=ORIENTED_EDGE('',*,*,#6853,.F.);
#8699=ORIENTED_EDGE('',*,*,#6852,.F.);
#8700=ORIENTED_EDGE('',*,*,#6854,.F.);
#8701=ORIENTED_EDGE('',*,*,#6855,.T.);
#8702=ORIENTED_EDGE('',*,*,#6856,.F.);
#8703=ORIENTED_EDGE('',*,*,#6855,.F.);
#8704=ORIENTED_EDGE('',*,*,#6857,.F.);
#8705=ORIENTED_EDGE('',*,*,#6858,.T.);
#8706=ORIENTED_EDGE('',*,*,#6859,.F.);
#8707=ORIENTED_EDGE('',*,*,#6860,.F.);
#8708=ORIENTED_EDGE('',*,*,#6861,.F.);
#8709=ORIENTED_EDGE('',*,*,#6862,.F.);
#8710=ORIENTED_EDGE('',*,*,#6863,.F.);
#8711=ORIENTED_EDGE('',*,*,#6864,.F.);
#8712=ORIENTED_EDGE('',*,*,#6865,.F.);
#8713=ORIENTED_EDGE('',*,*,#6866,.F.);
#8714=ORIENTED_EDGE('',*,*,#6867,.F.);
#8715=ORIENTED_EDGE('',*,*,#6862,.T.);
#8716=ORIENTED_EDGE('',*,*,#6868,.F.);
#8717=ORIENTED_EDGE('',*,*,#6869,.F.);
#8718=ORIENTED_EDGE('',*,*,#6870,.F.);
#8719=ORIENTED_EDGE('',*,*,#6858,.F.);
#8720=ORIENTED_EDGE('',*,*,#6860,.T.);
#8721=ORIENTED_EDGE('',*,*,#6871,.F.);
#8722=ORIENTED_EDGE('',*,*,#6872,.F.);
#8723=ORIENTED_EDGE('',*,*,#6873,.T.);
#8724=ORIENTED_EDGE('',*,*,#6864,.T.);
#8725=ORIENTED_EDGE('',*,*,#6874,.T.);
#8726=ORIENTED_EDGE('',*,*,#6875,.T.);
#8727=ORIENTED_EDGE('',*,*,#6876,.F.);
#8728=ORIENTED_EDGE('',*,*,#6859,.T.);
#8729=ORIENTED_EDGE('',*,*,#6870,.T.);
#8730=ORIENTED_EDGE('',*,*,#6877,.T.);
#8731=ORIENTED_EDGE('',*,*,#6865,.T.);
#8732=ORIENTED_EDGE('',*,*,#6861,.T.);
#8733=ORIENTED_EDGE('',*,*,#6876,.T.);
#8734=ORIENTED_EDGE('',*,*,#6878,.T.);
#8735=ORIENTED_EDGE('',*,*,#6879,.T.);
#8736=ORIENTED_EDGE('',*,*,#6880,.T.);
#8737=ORIENTED_EDGE('',*,*,#6871,.T.);
#8738=ORIENTED_EDGE('',*,*,#6853,.T.);
#8739=ORIENTED_EDGE('',*,*,#6856,.T.);
#8740=ORIENTED_EDGE('',*,*,#6869,.T.);
#8741=ORIENTED_EDGE('',*,*,#6881,.F.);
#8742=ORIENTED_EDGE('',*,*,#6866,.T.);
#8743=ORIENTED_EDGE('',*,*,#6877,.F.);
#8744=ORIENTED_EDGE('',*,*,#6882,.T.);
#8745=ORIENTED_EDGE('',*,*,#6872,.T.);
#8746=ORIENTED_EDGE('',*,*,#6880,.F.);
#8747=ORIENTED_EDGE('',*,*,#6883,.F.);
#8748=ORIENTED_EDGE('',*,*,#6884,.T.);
#8749=ORIENTED_EDGE('',*,*,#6883,.T.);
#8750=ORIENTED_EDGE('',*,*,#6879,.F.);
#8751=ORIENTED_EDGE('',*,*,#6885,.F.);
#8752=ORIENTED_EDGE('',*,*,#6886,.T.);
#8753=ORIENTED_EDGE('',*,*,#6885,.T.);
#8754=ORIENTED_EDGE('',*,*,#6878,.F.);
#8755=ORIENTED_EDGE('',*,*,#6875,.F.);
#8756=ORIENTED_EDGE('',*,*,#6857,.T.);
#8757=ORIENTED_EDGE('',*,*,#6873,.F.);
#8758=ORIENTED_EDGE('',*,*,#6882,.F.);
#8759=ORIENTED_EDGE('',*,*,#6884,.F.);
#8760=ORIENTED_EDGE('',*,*,#6886,.F.);
#8761=ORIENTED_EDGE('',*,*,#6874,.F.);
#8762=ORIENTED_EDGE('',*,*,#6863,.T.);
#8763=ORIENTED_EDGE('',*,*,#6867,.T.);
#8764=ORIENTED_EDGE('',*,*,#6881,.T.);
#8765=ORIENTED_EDGE('',*,*,#6868,.T.);
#8766=ORIENTED_EDGE('',*,*,#6851,.T.);
#8767=ORIENTED_EDGE('',*,*,#6854,.T.);
#8768=ORIENTED_EDGE('',*,*,#6887,.F.);
#8769=ORIENTED_EDGE('',*,*,#6888,.T.);
#8770=ORIENTED_EDGE('',*,*,#6889,.F.);
#8771=ORIENTED_EDGE('',*,*,#6890,.F.);
#8772=ORIENTED_EDGE('',*,*,#6891,.F.);
#8773=ORIENTED_EDGE('',*,*,#6892,.F.);
#8774=ORIENTED_EDGE('',*,*,#6893,.F.);
#8775=ORIENTED_EDGE('',*,*,#6894,.F.);
#8776=ORIENTED_EDGE('',*,*,#6895,.F.);
#8777=ORIENTED_EDGE('',*,*,#6896,.F.);
#8778=ORIENTED_EDGE('',*,*,#6897,.F.);
#8779=ORIENTED_EDGE('',*,*,#6898,.F.);
#8780=ORIENTED_EDGE('',*,*,#6899,.F.);
#8781=ORIENTED_EDGE('',*,*,#6892,.T.);
#8782=ORIENTED_EDGE('',*,*,#6900,.F.);
#8783=ORIENTED_EDGE('',*,*,#6901,.F.);
#8784=ORIENTED_EDGE('',*,*,#6902,.F.);
#8785=ORIENTED_EDGE('',*,*,#6903,.F.);
#8786=ORIENTED_EDGE('',*,*,#6904,.F.);
#8787=ORIENTED_EDGE('',*,*,#6888,.F.);
#8788=ORIENTED_EDGE('',*,*,#6893,.T.);
#8789=ORIENTED_EDGE('',*,*,#6899,.T.);
#8790=ORIENTED_EDGE('',*,*,#6905,.F.);
#8791=ORIENTED_EDGE('',*,*,#6900,.T.);
#8792=ORIENTED_EDGE('',*,*,#6887,.T.);
#8793=ORIENTED_EDGE('',*,*,#6906,.F.);
#8794=ORIENTED_EDGE('',*,*,#6894,.T.);
#8795=ORIENTED_EDGE('',*,*,#6906,.T.);
#8796=ORIENTED_EDGE('',*,*,#6890,.T.);
#8797=ORIENTED_EDGE('',*,*,#6907,.F.);
#8798=ORIENTED_EDGE('',*,*,#6898,.T.);
#8799=ORIENTED_EDGE('',*,*,#6908,.F.);
#8800=ORIENTED_EDGE('',*,*,#6901,.T.);
#8801=ORIENTED_EDGE('',*,*,#6905,.T.);
#8802=ORIENTED_EDGE('',*,*,#6897,.T.);
#8803=ORIENTED_EDGE('',*,*,#6909,.F.);
#8804=ORIENTED_EDGE('',*,*,#6902,.T.);
#8805=ORIENTED_EDGE('',*,*,#6908,.T.);
#8806=ORIENTED_EDGE('',*,*,#6896,.T.);
#8807=ORIENTED_EDGE('',*,*,#6910,.F.);
#8808=ORIENTED_EDGE('',*,*,#6903,.T.);
#8809=ORIENTED_EDGE('',*,*,#6909,.T.);
#8810=ORIENTED_EDGE('',*,*,#6891,.T.);
#8811=ORIENTED_EDGE('',*,*,#6907,.T.);
#8812=ORIENTED_EDGE('',*,*,#6889,.T.);
#8813=ORIENTED_EDGE('',*,*,#6904,.T.);
#8814=ORIENTED_EDGE('',*,*,#6910,.T.);
#8815=ORIENTED_EDGE('',*,*,#6895,.T.);
#8816=ORIENTED_EDGE('',*,*,#6911,.F.);
#8817=ORIENTED_EDGE('',*,*,#6912,.T.);
#8818=ORIENTED_EDGE('',*,*,#6913,.F.);
#8819=ORIENTED_EDGE('',*,*,#6912,.F.);
#8820=ORIENTED_EDGE('',*,*,#6914,.F.);
#8821=ORIENTED_EDGE('',*,*,#6915,.T.);
#8822=ORIENTED_EDGE('',*,*,#6916,.F.);
#8823=ORIENTED_EDGE('',*,*,#6915,.F.);
#8824=ORIENTED_EDGE('',*,*,#6917,.F.);
#8825=ORIENTED_EDGE('',*,*,#6918,.T.);
#8826=ORIENTED_EDGE('',*,*,#6919,.F.);
#8827=ORIENTED_EDGE('',*,*,#6920,.F.);
#8828=ORIENTED_EDGE('',*,*,#6921,.F.);
#8829=ORIENTED_EDGE('',*,*,#6922,.F.);
#8830=ORIENTED_EDGE('',*,*,#6923,.F.);
#8831=ORIENTED_EDGE('',*,*,#6924,.F.);
#8832=ORIENTED_EDGE('',*,*,#6925,.F.);
#8833=ORIENTED_EDGE('',*,*,#6926,.F.);
#8834=ORIENTED_EDGE('',*,*,#6927,.F.);
#8835=ORIENTED_EDGE('',*,*,#6922,.T.);
#8836=ORIENTED_EDGE('',*,*,#6928,.F.);
#8837=ORIENTED_EDGE('',*,*,#6929,.F.);
#8838=ORIENTED_EDGE('',*,*,#6930,.F.);
#8839=ORIENTED_EDGE('',*,*,#6918,.F.);
#8840=ORIENTED_EDGE('',*,*,#6920,.T.);
#8841=ORIENTED_EDGE('',*,*,#6931,.F.);
#8842=ORIENTED_EDGE('',*,*,#6932,.F.);
#8843=ORIENTED_EDGE('',*,*,#6933,.T.);
#8844=ORIENTED_EDGE('',*,*,#6924,.T.);
#8845=ORIENTED_EDGE('',*,*,#6934,.T.);
#8846=ORIENTED_EDGE('',*,*,#6935,.T.);
#8847=ORIENTED_EDGE('',*,*,#6936,.F.);
#8848=ORIENTED_EDGE('',*,*,#6919,.T.);
#8849=ORIENTED_EDGE('',*,*,#6930,.T.);
#8850=ORIENTED_EDGE('',*,*,#6937,.T.);
#8851=ORIENTED_EDGE('',*,*,#6925,.T.);
#8852=ORIENTED_EDGE('',*,*,#6921,.T.);
#8853=ORIENTED_EDGE('',*,*,#6936,.T.);
#8854=ORIENTED_EDGE('',*,*,#6938,.T.);
#8855=ORIENTED_EDGE('',*,*,#6939,.T.);
#8856=ORIENTED_EDGE('',*,*,#6940,.T.);
#8857=ORIENTED_EDGE('',*,*,#6931,.T.);
#8858=ORIENTED_EDGE('',*,*,#6913,.T.);
#8859=ORIENTED_EDGE('',*,*,#6916,.T.);
#8860=ORIENTED_EDGE('',*,*,#6929,.T.);
#8861=ORIENTED_EDGE('',*,*,#6941,.F.);
#8862=ORIENTED_EDGE('',*,*,#6926,.T.);
#8863=ORIENTED_EDGE('',*,*,#6937,.F.);
#8864=ORIENTED_EDGE('',*,*,#6942,.T.);
#8865=ORIENTED_EDGE('',*,*,#6932,.T.);
#8866=ORIENTED_EDGE('',*,*,#6940,.F.);
#8867=ORIENTED_EDGE('',*,*,#6943,.F.);
#8868=ORIENTED_EDGE('',*,*,#6944,.T.);
#8869=ORIENTED_EDGE('',*,*,#6943,.T.);
#8870=ORIENTED_EDGE('',*,*,#6939,.F.);
#8871=ORIENTED_EDGE('',*,*,#6945,.F.);
#8872=ORIENTED_EDGE('',*,*,#6946,.T.);
#8873=ORIENTED_EDGE('',*,*,#6945,.T.);
#8874=ORIENTED_EDGE('',*,*,#6938,.F.);
#8875=ORIENTED_EDGE('',*,*,#6935,.F.);
#8876=ORIENTED_EDGE('',*,*,#6917,.T.);
#8877=ORIENTED_EDGE('',*,*,#6933,.F.);
#8878=ORIENTED_EDGE('',*,*,#6942,.F.);
#8879=ORIENTED_EDGE('',*,*,#6944,.F.);
#8880=ORIENTED_EDGE('',*,*,#6946,.F.);
#8881=ORIENTED_EDGE('',*,*,#6934,.F.);
#8882=ORIENTED_EDGE('',*,*,#6923,.T.);
#8883=ORIENTED_EDGE('',*,*,#6927,.T.);
#8884=ORIENTED_EDGE('',*,*,#6941,.T.);
#8885=ORIENTED_EDGE('',*,*,#6928,.T.);
#8886=ORIENTED_EDGE('',*,*,#6911,.T.);
#8887=ORIENTED_EDGE('',*,*,#6914,.T.);
#8888=ORIENTED_EDGE('',*,*,#6947,.F.);
#8889=ORIENTED_EDGE('',*,*,#6948,.T.);
#8890=ORIENTED_EDGE('',*,*,#6949,.F.);
#8891=ORIENTED_EDGE('',*,*,#6948,.F.);
#8892=ORIENTED_EDGE('',*,*,#6947,.T.);
#8893=ORIENTED_EDGE('',*,*,#6950,.F.);
#8894=ORIENTED_EDGE('',*,*,#6951,.F.);
#8895=ORIENTED_EDGE('',*,*,#6952,.T.);
#8896=ORIENTED_EDGE('',*,*,#6953,.F.);
#8897=ORIENTED_EDGE('',*,*,#6952,.F.);
#8898=ORIENTED_EDGE('',*,*,#6951,.T.);
#8899=ORIENTED_EDGE('',*,*,#6954,.F.);
#8900=ORIENTED_EDGE('',*,*,#6955,.F.);
#8901=ORIENTED_EDGE('',*,*,#6956,.T.);
#8902=ORIENTED_EDGE('',*,*,#6950,.T.);
#8903=ORIENTED_EDGE('',*,*,#6956,.F.);
#8904=ORIENTED_EDGE('',*,*,#6957,.F.);
#8905=ORIENTED_EDGE('',*,*,#6958,.T.);
#8906=ORIENTED_EDGE('',*,*,#6954,.T.);
#8907=ORIENTED_EDGE('',*,*,#6958,.F.);
#8908=ORIENTED_EDGE('',*,*,#6959,.F.);
#8909=ORIENTED_EDGE('',*,*,#6960,.T.);
#8910=ORIENTED_EDGE('',*,*,#6961,.T.);
#8911=ORIENTED_EDGE('',*,*,#6960,.F.);
#8912=ORIENTED_EDGE('',*,*,#6959,.T.);
#8913=ORIENTED_EDGE('',*,*,#6949,.T.);
#8914=ORIENTED_EDGE('',*,*,#6953,.T.);
#8915=ORIENTED_EDGE('',*,*,#6961,.F.);
#8916=ORIENTED_EDGE('',*,*,#6955,.T.);
#8917=ORIENTED_EDGE('',*,*,#6957,.T.);
#8918=ORIENTED_EDGE('',*,*,#6962,.F.);
#8919=ORIENTED_EDGE('',*,*,#6963,.F.);
#8920=ORIENTED_EDGE('',*,*,#6964,.F.);
#8921=ORIENTED_EDGE('',*,*,#6965,.F.);
#8922=ORIENTED_EDGE('',*,*,#6964,.T.);
#8923=ORIENTED_EDGE('',*,*,#6966,.F.);
#8924=ORIENTED_EDGE('',*,*,#6967,.F.);
#8925=ORIENTED_EDGE('',*,*,#6968,.T.);
#8926=ORIENTED_EDGE('',*,*,#6969,.F.);
#8927=ORIENTED_EDGE('',*,*,#6970,.T.);
#8928=ORIENTED_EDGE('',*,*,#6971,.T.);
#8929=ORIENTED_EDGE('',*,*,#6963,.T.);
#8930=ORIENTED_EDGE('',*,*,#6972,.F.);
#8931=ORIENTED_EDGE('',*,*,#6973,.F.);
#8932=ORIENTED_EDGE('',*,*,#6966,.T.);
#8933=ORIENTED_EDGE('',*,*,#6974,.F.);
#8934=ORIENTED_EDGE('',*,*,#6975,.T.);
#8935=ORIENTED_EDGE('',*,*,#6976,.F.);
#8936=ORIENTED_EDGE('',*,*,#6975,.F.);
#8937=ORIENTED_EDGE('',*,*,#6977,.F.);
#8938=ORIENTED_EDGE('',*,*,#6978,.T.);
#8939=ORIENTED_EDGE('',*,*,#6979,.F.);
#8940=ORIENTED_EDGE('',*,*,#6978,.F.);
#8941=ORIENTED_EDGE('',*,*,#6980,.F.);
#8942=ORIENTED_EDGE('',*,*,#6981,.T.);
#8943=ORIENTED_EDGE('',*,*,#6982,.F.);
#8944=ORIENTED_EDGE('',*,*,#6981,.F.);
#8945=ORIENTED_EDGE('',*,*,#6983,.F.);
#8946=ORIENTED_EDGE('',*,*,#6984,.T.);
#8947=ORIENTED_EDGE('',*,*,#6985,.F.);
#8948=ORIENTED_EDGE('',*,*,#6984,.F.);
#8949=ORIENTED_EDGE('',*,*,#6971,.F.);
#8950=ORIENTED_EDGE('',*,*,#6986,.T.);
#8951=ORIENTED_EDGE('',*,*,#6987,.F.);
#8952=ORIENTED_EDGE('',*,*,#6986,.F.);
#8953=ORIENTED_EDGE('',*,*,#6970,.F.);
#8954=ORIENTED_EDGE('',*,*,#6988,.T.);
#8955=ORIENTED_EDGE('',*,*,#6989,.F.);
#8956=ORIENTED_EDGE('',*,*,#6988,.F.);
#8957=ORIENTED_EDGE('',*,*,#6990,.F.);
#8958=ORIENTED_EDGE('',*,*,#6991,.T.);
#8959=ORIENTED_EDGE('',*,*,#6992,.F.);
#8960=ORIENTED_EDGE('',*,*,#6991,.F.);
#8961=ORIENTED_EDGE('',*,*,#6962,.T.);
#8962=ORIENTED_EDGE('',*,*,#6993,.F.);
#8963=ORIENTED_EDGE('',*,*,#6994,.F.);
#8964=ORIENTED_EDGE('',*,*,#6995,.F.);
#8965=ORIENTED_EDGE('',*,*,#6972,.T.);
#8966=ORIENTED_EDGE('',*,*,#6989,.T.);
#8967=ORIENTED_EDGE('',*,*,#6996,.F.);
#8968=ORIENTED_EDGE('',*,*,#6997,.F.);
#8969=ORIENTED_EDGE('',*,*,#6998,.F.);
#8970=ORIENTED_EDGE('',*,*,#6999,.F.);
#8971=ORIENTED_EDGE('',*,*,#6987,.T.);
#8972=ORIENTED_EDGE('',*,*,#7000,.F.);
#8973=ORIENTED_EDGE('',*,*,#6998,.T.);
#8974=ORIENTED_EDGE('',*,*,#7001,.F.);
#8975=ORIENTED_EDGE('',*,*,#6968,.F.);
#8976=ORIENTED_EDGE('',*,*,#7002,.T.);
#8977=ORIENTED_EDGE('',*,*,#7003,.F.);
#8978=ORIENTED_EDGE('',*,*,#7004,.F.);
#8979=ORIENTED_EDGE('',*,*,#6999,.T.);
#8980=ORIENTED_EDGE('',*,*,#7000,.T.);
#8981=ORIENTED_EDGE('',*,*,#6967,.T.);
#8982=ORIENTED_EDGE('',*,*,#6973,.T.);
#8983=ORIENTED_EDGE('',*,*,#6995,.T.);
#8984=ORIENTED_EDGE('',*,*,#6990,.T.);
#8985=ORIENTED_EDGE('',*,*,#6983,.T.);
#8986=ORIENTED_EDGE('',*,*,#6980,.T.);
#8987=ORIENTED_EDGE('',*,*,#6977,.T.);
#8988=ORIENTED_EDGE('',*,*,#6974,.T.);
#8989=ORIENTED_EDGE('',*,*,#6994,.T.);
#8990=ORIENTED_EDGE('',*,*,#7005,.T.);
#8991=ORIENTED_EDGE('',*,*,#7006,.F.);
#8992=ORIENTED_EDGE('',*,*,#7002,.F.);
#8993=ORIENTED_EDGE('',*,*,#6965,.T.);
#8994=ORIENTED_EDGE('',*,*,#6969,.T.);
#8995=ORIENTED_EDGE('',*,*,#7001,.T.);
#8996=ORIENTED_EDGE('',*,*,#6997,.T.);
#8997=ORIENTED_EDGE('',*,*,#7007,.T.);
#8998=ORIENTED_EDGE('',*,*,#7008,.F.);
#8999=ORIENTED_EDGE('',*,*,#7005,.F.);
#9000=ORIENTED_EDGE('',*,*,#6993,.T.);
#9001=ORIENTED_EDGE('',*,*,#6992,.T.);
#9002=ORIENTED_EDGE('',*,*,#6985,.T.);
#9003=ORIENTED_EDGE('',*,*,#6982,.T.);
#9004=ORIENTED_EDGE('',*,*,#6979,.T.);
#9005=ORIENTED_EDGE('',*,*,#6976,.T.);
#9006=ORIENTED_EDGE('',*,*,#6996,.T.);
#9007=ORIENTED_EDGE('',*,*,#7004,.T.);
#9008=ORIENTED_EDGE('',*,*,#7009,.F.);
#9009=ORIENTED_EDGE('',*,*,#7007,.F.);
#9010=ORIENTED_EDGE('',*,*,#7009,.T.);
#9011=ORIENTED_EDGE('',*,*,#7003,.T.);
#9012=ORIENTED_EDGE('',*,*,#7006,.T.);
#9013=ORIENTED_EDGE('',*,*,#7008,.T.);
#9014=ORIENTED_EDGE('',*,*,#7010,.F.);
#9015=ORIENTED_EDGE('',*,*,#7011,.T.);
#9016=ORIENTED_EDGE('',*,*,#7012,.F.);
#9017=ORIENTED_EDGE('',*,*,#7011,.F.);
#9018=ORIENTED_EDGE('',*,*,#7013,.F.);
#9019=ORIENTED_EDGE('',*,*,#7014,.T.);
#9020=ORIENTED_EDGE('',*,*,#7015,.F.);
#9021=ORIENTED_EDGE('',*,*,#7014,.F.);
#9022=ORIENTED_EDGE('',*,*,#7016,.F.);
#9023=ORIENTED_EDGE('',*,*,#7017,.T.);
#9024=ORIENTED_EDGE('',*,*,#7018,.F.);
#9025=ORIENTED_EDGE('',*,*,#7017,.F.);
#9026=ORIENTED_EDGE('',*,*,#7019,.F.);
#9027=ORIENTED_EDGE('',*,*,#7020,.T.);
#9028=ORIENTED_EDGE('',*,*,#7021,.F.);
#9029=ORIENTED_EDGE('',*,*,#7020,.F.);
#9030=ORIENTED_EDGE('',*,*,#7022,.F.);
#9031=ORIENTED_EDGE('',*,*,#7023,.T.);
#9032=ORIENTED_EDGE('',*,*,#7024,.F.);
#9033=ORIENTED_EDGE('',*,*,#7023,.F.);
#9034=ORIENTED_EDGE('',*,*,#7025,.F.);
#9035=ORIENTED_EDGE('',*,*,#7026,.T.);
#9036=ORIENTED_EDGE('',*,*,#7027,.F.);
#9037=ORIENTED_EDGE('',*,*,#7026,.F.);
#9038=ORIENTED_EDGE('',*,*,#7025,.T.);
#9039=ORIENTED_EDGE('',*,*,#7012,.T.);
#9040=ORIENTED_EDGE('',*,*,#7028,.F.);
#9041=ORIENTED_EDGE('',*,*,#7029,.T.);
#9042=ORIENTED_EDGE('',*,*,#7030,.T.);
#9043=ORIENTED_EDGE('',*,*,#7029,.F.);
#9044=ORIENTED_EDGE('',*,*,#7028,.T.);
#9045=ORIENTED_EDGE('',*,*,#7027,.T.);
#9046=ORIENTED_EDGE('',*,*,#7024,.T.);
#9047=ORIENTED_EDGE('',*,*,#7021,.T.);
#9048=ORIENTED_EDGE('',*,*,#7018,.T.);
#9049=ORIENTED_EDGE('',*,*,#7015,.T.);
#9050=ORIENTED_EDGE('',*,*,#7030,.F.);
#9051=ORIENTED_EDGE('',*,*,#7010,.T.);
#9052=ORIENTED_EDGE('',*,*,#7022,.T.);
#9053=ORIENTED_EDGE('',*,*,#7019,.T.);
#9054=ORIENTED_EDGE('',*,*,#7016,.T.);
#9055=ORIENTED_EDGE('',*,*,#7013,.T.);
#9056=ORIENTED_EDGE('',*,*,#7031,.F.);
#9057=ORIENTED_EDGE('',*,*,#7032,.T.);
#9058=ORIENTED_EDGE('',*,*,#7033,.F.);
#9059=ORIENTED_EDGE('',*,*,#7032,.F.);
#9060=ORIENTED_EDGE('',*,*,#7034,.F.);
#9061=ORIENTED_EDGE('',*,*,#7035,.T.);
#9062=ORIENTED_EDGE('',*,*,#7036,.F.);
#9063=ORIENTED_EDGE('',*,*,#7035,.F.);
#9064=ORIENTED_EDGE('',*,*,#7037,.F.);
#9065=ORIENTED_EDGE('',*,*,#7038,.T.);
#9066=ORIENTED_EDGE('',*,*,#7039,.F.);
#9067=ORIENTED_EDGE('',*,*,#7038,.F.);
#9068=ORIENTED_EDGE('',*,*,#7040,.F.);
#9069=ORIENTED_EDGE('',*,*,#7041,.T.);
#9070=ORIENTED_EDGE('',*,*,#7042,.F.);
#9071=ORIENTED_EDGE('',*,*,#7041,.F.);
#9072=ORIENTED_EDGE('',*,*,#7043,.F.);
#9073=ORIENTED_EDGE('',*,*,#7044,.T.);
#9074=ORIENTED_EDGE('',*,*,#7045,.F.);
#9075=ORIENTED_EDGE('',*,*,#7044,.F.);
#9076=ORIENTED_EDGE('',*,*,#7046,.F.);
#9077=ORIENTED_EDGE('',*,*,#7047,.T.);
#9078=ORIENTED_EDGE('',*,*,#7048,.T.);
#9079=ORIENTED_EDGE('',*,*,#7047,.F.);
#9080=ORIENTED_EDGE('',*,*,#7048,.F.);
#9081=ORIENTED_EDGE('',*,*,#7031,.T.);
#9082=ORIENTED_EDGE('',*,*,#7049,.F.);
#9083=ORIENTED_EDGE('',*,*,#7050,.T.);
#9084=ORIENTED_EDGE('',*,*,#7051,.T.);
#9085=ORIENTED_EDGE('',*,*,#7050,.F.);
#9086=ORIENTED_EDGE('',*,*,#7049,.T.);
#9087=ORIENTED_EDGE('',*,*,#7033,.T.);
#9088=ORIENTED_EDGE('',*,*,#7045,.T.);
#9089=ORIENTED_EDGE('',*,*,#7042,.T.);
#9090=ORIENTED_EDGE('',*,*,#7039,.T.);
#9091=ORIENTED_EDGE('',*,*,#7036,.T.);
#9092=ORIENTED_EDGE('',*,*,#7051,.F.);
#9093=ORIENTED_EDGE('',*,*,#7046,.T.);
#9094=ORIENTED_EDGE('',*,*,#7043,.T.);
#9095=ORIENTED_EDGE('',*,*,#7040,.T.);
#9096=ORIENTED_EDGE('',*,*,#7037,.T.);
#9097=ORIENTED_EDGE('',*,*,#7034,.T.);
#9098=ORIENTED_EDGE('',*,*,#7052,.F.);
#9099=ORIENTED_EDGE('',*,*,#7053,.F.);
#9100=ORIENTED_EDGE('',*,*,#7054,.F.);
#9101=ORIENTED_EDGE('',*,*,#7055,.F.);
#9102=ORIENTED_EDGE('',*,*,#7054,.T.);
#9103=ORIENTED_EDGE('',*,*,#7056,.F.);
#9104=ORIENTED_EDGE('',*,*,#7057,.T.);
#9105=ORIENTED_EDGE('',*,*,#7058,.F.);
#9106=ORIENTED_EDGE('',*,*,#7059,.F.);
#9107=ORIENTED_EDGE('',*,*,#7060,.T.);
#9108=ORIENTED_EDGE('',*,*,#7061,.T.);
#9109=ORIENTED_EDGE('',*,*,#7053,.T.);
#9110=ORIENTED_EDGE('',*,*,#7062,.T.);
#9111=ORIENTED_EDGE('',*,*,#7063,.T.);
#9112=ORIENTED_EDGE('',*,*,#7064,.F.);
#9113=ORIENTED_EDGE('',*,*,#7065,.F.);
#9114=ORIENTED_EDGE('',*,*,#7066,.T.);
#9115=ORIENTED_EDGE('',*,*,#7067,.T.);
#9116=ORIENTED_EDGE('',*,*,#7056,.T.);
#9117=ORIENTED_EDGE('',*,*,#7068,.T.);
#9118=ORIENTED_EDGE('',*,*,#7069,.T.);
#9119=ORIENTED_EDGE('',*,*,#7070,.T.);
#9120=ORIENTED_EDGE('',*,*,#7071,.T.);
#9121=ORIENTED_EDGE('',*,*,#7072,.T.);
#9122=ORIENTED_EDGE('',*,*,#7068,.F.);
#9123=ORIENTED_EDGE('',*,*,#7073,.T.);
#9124=ORIENTED_EDGE('',*,*,#7074,.F.);
#9125=ORIENTED_EDGE('',*,*,#7073,.F.);
#9126=ORIENTED_EDGE('',*,*,#7069,.F.);
#9127=ORIENTED_EDGE('',*,*,#7075,.T.);
#9128=ORIENTED_EDGE('',*,*,#7076,.F.);
#9129=ORIENTED_EDGE('',*,*,#7075,.F.);
#9130=ORIENTED_EDGE('',*,*,#7070,.F.);
#9131=ORIENTED_EDGE('',*,*,#7077,.T.);
#9132=ORIENTED_EDGE('',*,*,#7078,.F.);
#9133=ORIENTED_EDGE('',*,*,#7077,.F.);
#9134=ORIENTED_EDGE('',*,*,#7071,.F.);
#9135=ORIENTED_EDGE('',*,*,#7079,.T.);
#9136=ORIENTED_EDGE('',*,*,#7080,.F.);
#9137=ORIENTED_EDGE('',*,*,#7079,.F.);
#9138=ORIENTED_EDGE('',*,*,#7061,.F.);
#9139=ORIENTED_EDGE('',*,*,#7081,.T.);
#9140=ORIENTED_EDGE('',*,*,#7082,.F.);
#9141=ORIENTED_EDGE('',*,*,#7081,.F.);
#9142=ORIENTED_EDGE('',*,*,#7060,.F.);
#9143=ORIENTED_EDGE('',*,*,#7083,.T.);
#9144=ORIENTED_EDGE('',*,*,#7084,.F.);
#9145=ORIENTED_EDGE('',*,*,#7083,.F.);
#9146=ORIENTED_EDGE('',*,*,#7072,.F.);
#9147=ORIENTED_EDGE('',*,*,#7085,.T.);
#9148=ORIENTED_EDGE('',*,*,#7086,.F.);
#9149=ORIENTED_EDGE('',*,*,#7085,.F.);
#9150=ORIENTED_EDGE('',*,*,#7052,.T.);
#9151=ORIENTED_EDGE('',*,*,#7087,.T.);
#9152=ORIENTED_EDGE('',*,*,#7088,.F.);
#9153=ORIENTED_EDGE('',*,*,#7089,.F.);
#9154=ORIENTED_EDGE('',*,*,#7062,.F.);
#9155=ORIENTED_EDGE('',*,*,#7084,.T.);
#9156=ORIENTED_EDGE('',*,*,#7090,.F.);
#9157=ORIENTED_EDGE('',*,*,#7091,.F.);
#9158=ORIENTED_EDGE('',*,*,#7092,.F.);
#9159=ORIENTED_EDGE('',*,*,#7066,.F.);
#9160=ORIENTED_EDGE('',*,*,#7082,.T.);
#9161=ORIENTED_EDGE('',*,*,#7067,.F.);
#9162=ORIENTED_EDGE('',*,*,#7092,.T.);
#9163=ORIENTED_EDGE('',*,*,#7093,.F.);
#9164=ORIENTED_EDGE('',*,*,#7057,.F.);
#9165=ORIENTED_EDGE('',*,*,#7055,.T.);
#9166=ORIENTED_EDGE('',*,*,#7059,.T.);
#9167=ORIENTED_EDGE('',*,*,#7094,.F.);
#9168=ORIENTED_EDGE('',*,*,#7087,.F.);
#9169=ORIENTED_EDGE('',*,*,#7089,.T.);
#9170=ORIENTED_EDGE('',*,*,#7095,.T.);
#9171=ORIENTED_EDGE('',*,*,#7096,.F.);
#9172=ORIENTED_EDGE('',*,*,#7063,.F.);
#9173=ORIENTED_EDGE('',*,*,#7097,.T.);
#9174=ORIENTED_EDGE('',*,*,#7098,.F.);
#9175=ORIENTED_EDGE('',*,*,#7095,.F.);
#9176=ORIENTED_EDGE('',*,*,#7088,.T.);
#9177=ORIENTED_EDGE('',*,*,#7094,.T.);
#9178=ORIENTED_EDGE('',*,*,#7058,.T.);
#9179=ORIENTED_EDGE('',*,*,#7093,.T.);
#9180=ORIENTED_EDGE('',*,*,#7091,.T.);
#9181=ORIENTED_EDGE('',*,*,#7086,.T.);
#9182=ORIENTED_EDGE('',*,*,#7080,.T.);
#9183=ORIENTED_EDGE('',*,*,#7078,.T.);
#9184=ORIENTED_EDGE('',*,*,#7076,.T.);
#9185=ORIENTED_EDGE('',*,*,#7074,.T.);
#9186=ORIENTED_EDGE('',*,*,#7090,.T.);
#9187=ORIENTED_EDGE('',*,*,#7065,.T.);
#9188=ORIENTED_EDGE('',*,*,#7099,.F.);
#9189=ORIENTED_EDGE('',*,*,#7097,.F.);
#9190=ORIENTED_EDGE('',*,*,#7099,.T.);
#9191=ORIENTED_EDGE('',*,*,#7064,.T.);
#9192=ORIENTED_EDGE('',*,*,#7096,.T.);
#9193=ORIENTED_EDGE('',*,*,#7098,.T.);
#9194=ORIENTED_EDGE('',*,*,#7100,.F.);
#9195=ORIENTED_EDGE('',*,*,#7101,.T.);
#9196=ORIENTED_EDGE('',*,*,#7102,.F.);
#9197=ORIENTED_EDGE('',*,*,#7101,.F.);
#9198=ORIENTED_EDGE('',*,*,#7103,.F.);
#9199=ORIENTED_EDGE('',*,*,#7104,.T.);
#9200=ORIENTED_EDGE('',*,*,#7105,.F.);
#9201=ORIENTED_EDGE('',*,*,#7104,.F.);
#9202=ORIENTED_EDGE('',*,*,#7106,.F.);
#9203=ORIENTED_EDGE('',*,*,#7107,.T.);
#9204=ORIENTED_EDGE('',*,*,#7108,.F.);
#9205=ORIENTED_EDGE('',*,*,#7107,.F.);
#9206=ORIENTED_EDGE('',*,*,#7109,.F.);
#9207=ORIENTED_EDGE('',*,*,#7110,.T.);
#9208=ORIENTED_EDGE('',*,*,#7111,.F.);
#9209=ORIENTED_EDGE('',*,*,#7110,.F.);
#9210=ORIENTED_EDGE('',*,*,#7112,.F.);
#9211=ORIENTED_EDGE('',*,*,#7113,.T.);
#9212=ORIENTED_EDGE('',*,*,#7114,.F.);
#9213=ORIENTED_EDGE('',*,*,#7113,.F.);
#9214=ORIENTED_EDGE('',*,*,#7115,.F.);
#9215=ORIENTED_EDGE('',*,*,#7116,.T.);
#9216=ORIENTED_EDGE('',*,*,#7117,.F.);
#9217=ORIENTED_EDGE('',*,*,#7116,.F.);
#9218=ORIENTED_EDGE('',*,*,#7115,.T.);
#9219=ORIENTED_EDGE('',*,*,#7102,.T.);
#9220=ORIENTED_EDGE('',*,*,#7118,.F.);
#9221=ORIENTED_EDGE('',*,*,#7119,.T.);
#9222=ORIENTED_EDGE('',*,*,#7120,.T.);
#9223=ORIENTED_EDGE('',*,*,#7119,.F.);
#9224=ORIENTED_EDGE('',*,*,#7118,.T.);
#9225=ORIENTED_EDGE('',*,*,#7117,.T.);
#9226=ORIENTED_EDGE('',*,*,#7114,.T.);
#9227=ORIENTED_EDGE('',*,*,#7111,.T.);
#9228=ORIENTED_EDGE('',*,*,#7108,.T.);
#9229=ORIENTED_EDGE('',*,*,#7105,.T.);
#9230=ORIENTED_EDGE('',*,*,#7120,.F.);
#9231=ORIENTED_EDGE('',*,*,#7100,.T.);
#9232=ORIENTED_EDGE('',*,*,#7112,.T.);
#9233=ORIENTED_EDGE('',*,*,#7109,.T.);
#9234=ORIENTED_EDGE('',*,*,#7106,.T.);
#9235=ORIENTED_EDGE('',*,*,#7103,.T.);
#9236=ORIENTED_EDGE('',*,*,#7121,.F.);
#9237=ORIENTED_EDGE('',*,*,#7122,.T.);
#9238=ORIENTED_EDGE('',*,*,#7123,.F.);
#9239=ORIENTED_EDGE('',*,*,#7122,.F.);
#9240=ORIENTED_EDGE('',*,*,#7124,.F.);
#9241=ORIENTED_EDGE('',*,*,#7125,.T.);
#9242=ORIENTED_EDGE('',*,*,#7126,.F.);
#9243=ORIENTED_EDGE('',*,*,#7125,.F.);
#9244=ORIENTED_EDGE('',*,*,#7127,.F.);
#9245=ORIENTED_EDGE('',*,*,#7128,.T.);
#9246=ORIENTED_EDGE('',*,*,#7129,.F.);
#9247=ORIENTED_EDGE('',*,*,#7128,.F.);
#9248=ORIENTED_EDGE('',*,*,#7130,.F.);
#9249=ORIENTED_EDGE('',*,*,#7131,.T.);
#9250=ORIENTED_EDGE('',*,*,#7132,.F.);
#9251=ORIENTED_EDGE('',*,*,#7131,.F.);
#9252=ORIENTED_EDGE('',*,*,#7133,.F.);
#9253=ORIENTED_EDGE('',*,*,#7134,.T.);
#9254=ORIENTED_EDGE('',*,*,#7135,.F.);
#9255=ORIENTED_EDGE('',*,*,#7134,.F.);
#9256=ORIENTED_EDGE('',*,*,#7136,.F.);
#9257=ORIENTED_EDGE('',*,*,#7137,.T.);
#9258=ORIENTED_EDGE('',*,*,#7138,.T.);
#9259=ORIENTED_EDGE('',*,*,#7137,.F.);
#9260=ORIENTED_EDGE('',*,*,#7138,.F.);
#9261=ORIENTED_EDGE('',*,*,#7121,.T.);
#9262=ORIENTED_EDGE('',*,*,#7139,.F.);
#9263=ORIENTED_EDGE('',*,*,#7140,.T.);
#9264=ORIENTED_EDGE('',*,*,#7141,.T.);
#9265=ORIENTED_EDGE('',*,*,#7140,.F.);
#9266=ORIENTED_EDGE('',*,*,#7139,.T.);
#9267=ORIENTED_EDGE('',*,*,#7123,.T.);
#9268=ORIENTED_EDGE('',*,*,#7135,.T.);
#9269=ORIENTED_EDGE('',*,*,#7132,.T.);
#9270=ORIENTED_EDGE('',*,*,#7129,.T.);
#9271=ORIENTED_EDGE('',*,*,#7126,.T.);
#9272=ORIENTED_EDGE('',*,*,#7141,.F.);
#9273=ORIENTED_EDGE('',*,*,#7136,.T.);
#9274=ORIENTED_EDGE('',*,*,#7133,.T.);
#9275=ORIENTED_EDGE('',*,*,#7130,.T.);
#9276=ORIENTED_EDGE('',*,*,#7127,.T.);
#9277=ORIENTED_EDGE('',*,*,#7124,.T.);
#9278=ORIENTED_EDGE('',*,*,#7142,.F.);
#9279=ORIENTED_EDGE('',*,*,#7143,.F.);
#9280=ORIENTED_EDGE('',*,*,#7144,.T.);
#9281=ORIENTED_EDGE('',*,*,#7142,.T.);
#9282=ORIENTED_EDGE('',*,*,#7144,.F.);
#9283=ORIENTED_EDGE('',*,*,#7145,.F.);
#9284=ORIENTED_EDGE('',*,*,#7146,.T.);
#9285=ORIENTED_EDGE('',*,*,#7143,.T.);
#9286=ORIENTED_EDGE('',*,*,#7146,.F.);
#9287=ORIENTED_EDGE('',*,*,#7147,.F.);
#9288=ORIENTED_EDGE('',*,*,#7148,.T.);
#9289=ORIENTED_EDGE('',*,*,#7145,.T.);
#9290=ORIENTED_EDGE('',*,*,#7148,.F.);
#9291=ORIENTED_EDGE('',*,*,#7147,.T.);
#9292=ORIENTED_EDGE('',*,*,#7149,.F.);
#9293=ORIENTED_EDGE('',*,*,#7150,.F.);
#9294=ORIENTED_EDGE('',*,*,#7151,.T.);
#9295=ORIENTED_EDGE('',*,*,#7149,.T.);
#9296=ORIENTED_EDGE('',*,*,#7151,.F.);
#9297=ORIENTED_EDGE('',*,*,#7152,.F.);
#9298=ORIENTED_EDGE('',*,*,#7153,.T.);
#9299=ORIENTED_EDGE('',*,*,#7150,.T.);
#9300=ORIENTED_EDGE('',*,*,#7153,.F.);
#9301=ORIENTED_EDGE('',*,*,#7154,.F.);
#9302=ORIENTED_EDGE('',*,*,#7155,.T.);
#9303=ORIENTED_EDGE('',*,*,#7152,.T.);
#9304=ORIENTED_EDGE('',*,*,#7155,.F.);
#9305=ORIENTED_EDGE('',*,*,#7154,.T.);
#9306=ORIENTED_EDGE('',*,*,#7156,.T.);
#9307=ORIENTED_EDGE('',*,*,#7157,.T.);
#9308=ORIENTED_EDGE('',*,*,#7158,.T.);
#9309=ORIENTED_EDGE('',*,*,#7159,.F.);
#9310=ORIENTED_EDGE('',*,*,#7160,.T.);
#9311=ORIENTED_EDGE('',*,*,#7161,.T.);
#9312=ORIENTED_EDGE('',*,*,#7162,.T.);
#9313=ORIENTED_EDGE('',*,*,#7157,.F.);
#9314=ORIENTED_EDGE('',*,*,#7163,.T.);
#9315=ORIENTED_EDGE('',*,*,#7164,.T.);
#9316=ORIENTED_EDGE('',*,*,#7165,.T.);
#9317=ORIENTED_EDGE('',*,*,#7161,.F.);
#9318=ORIENTED_EDGE('',*,*,#7166,.T.);
#9319=ORIENTED_EDGE('',*,*,#7167,.T.);
#9320=ORIENTED_EDGE('',*,*,#7168,.T.);
#9321=ORIENTED_EDGE('',*,*,#7164,.F.);
#9322=ORIENTED_EDGE('',*,*,#7169,.T.);
#9323=ORIENTED_EDGE('',*,*,#7170,.T.);
#9324=ORIENTED_EDGE('',*,*,#7171,.T.);
#9325=ORIENTED_EDGE('',*,*,#7167,.F.);
#9326=ORIENTED_EDGE('',*,*,#7172,.T.);
#9327=ORIENTED_EDGE('',*,*,#7159,.T.);
#9328=ORIENTED_EDGE('',*,*,#7173,.T.);
#9329=ORIENTED_EDGE('',*,*,#7170,.F.);
#9330=ORIENTED_EDGE('',*,*,#7172,.F.);
#9331=ORIENTED_EDGE('',*,*,#7169,.F.);
#9332=ORIENTED_EDGE('',*,*,#7166,.F.);
#9333=ORIENTED_EDGE('',*,*,#7163,.F.);
#9334=ORIENTED_EDGE('',*,*,#7160,.F.);
#9335=ORIENTED_EDGE('',*,*,#7156,.F.);
#9336=ORIENTED_EDGE('',*,*,#7173,.F.);
#9337=ORIENTED_EDGE('',*,*,#7158,.F.);
#9338=ORIENTED_EDGE('',*,*,#7162,.F.);
#9339=ORIENTED_EDGE('',*,*,#7165,.F.);
#9340=ORIENTED_EDGE('',*,*,#7168,.F.);
#9341=ORIENTED_EDGE('',*,*,#7171,.F.);
#9342=ORIENTED_EDGE('',*,*,#7174,.F.);
#9343=ORIENTED_EDGE('',*,*,#7175,.F.);
#9344=ORIENTED_EDGE('',*,*,#7176,.T.);
#9345=ORIENTED_EDGE('',*,*,#7177,.F.);
#9346=ORIENTED_EDGE('',*,*,#7178,.F.);
#9347=ORIENTED_EDGE('',*,*,#7176,.F.);
#9348=ORIENTED_EDGE('',*,*,#7177,.T.);
#9349=ORIENTED_EDGE('',*,*,#7178,.T.);
#9350=ORIENTED_EDGE('',*,*,#7179,.T.);
#9351=ORIENTED_EDGE('',*,*,#7180,.T.);
#9352=ORIENTED_EDGE('',*,*,#7179,.F.);
#9353=ORIENTED_EDGE('',*,*,#7181,.T.);
#9354=ORIENTED_EDGE('',*,*,#7182,.T.);
#9355=ORIENTED_EDGE('',*,*,#7183,.F.);
#9356=ORIENTED_EDGE('',*,*,#7182,.F.);
#9357=ORIENTED_EDGE('',*,*,#7183,.T.);
#9358=ORIENTED_EDGE('',*,*,#7184,.T.);
#9359=ORIENTED_EDGE('',*,*,#7185,.F.);
#9360=ORIENTED_EDGE('',*,*,#7184,.F.);
#9361=ORIENTED_EDGE('',*,*,#7180,.F.);
#9362=ORIENTED_EDGE('',*,*,#7185,.T.);
#9363=ORIENTED_EDGE('',*,*,#7186,.F.);
#9364=ORIENTED_EDGE('',*,*,#7187,.T.);
#9365=ORIENTED_EDGE('',*,*,#7174,.T.);
#9366=ORIENTED_EDGE('',*,*,#7175,.T.);
#9367=ORIENTED_EDGE('',*,*,#7187,.F.);
#9368=ORIENTED_EDGE('',*,*,#7186,.T.);
#9369=ORIENTED_EDGE('',*,*,#7188,.F.);
#9370=ORIENTED_EDGE('',*,*,#7188,.T.);
#9371=ORIENTED_EDGE('',*,*,#7189,.T.);
#9372=ORIENTED_EDGE('',*,*,#7181,.F.);
#9373=ORIENTED_EDGE('',*,*,#7189,.F.);
#9374=ORIENTED_EDGE('',*,*,#7190,.F.);
#9375=ORIENTED_EDGE('',*,*,#7191,.F.);
#9376=ORIENTED_EDGE('',*,*,#7192,.T.);
#9377=ORIENTED_EDGE('',*,*,#7193,.F.);
#9378=ORIENTED_EDGE('',*,*,#7194,.F.);
#9379=ORIENTED_EDGE('',*,*,#7192,.F.);
#9380=ORIENTED_EDGE('',*,*,#7195,.T.);
#9381=ORIENTED_EDGE('',*,*,#7196,.T.);
#9382=ORIENTED_EDGE('',*,*,#7193,.T.);
#9383=ORIENTED_EDGE('',*,*,#7194,.T.);
#9384=ORIENTED_EDGE('',*,*,#7196,.F.);
#9385=ORIENTED_EDGE('',*,*,#7197,.F.);
#9386=ORIENTED_EDGE('',*,*,#7198,.T.);
#9387=ORIENTED_EDGE('',*,*,#7199,.F.);
#9388=ORIENTED_EDGE('',*,*,#7200,.T.);
#9389=ORIENTED_EDGE('',*,*,#7197,.T.);
#9390=ORIENTED_EDGE('',*,*,#7200,.F.);
#9391=ORIENTED_EDGE('',*,*,#7201,.F.);
#9392=ORIENTED_EDGE('',*,*,#7202,.T.);
#9393=ORIENTED_EDGE('',*,*,#7199,.T.);
#9394=ORIENTED_EDGE('',*,*,#7202,.F.);
#9395=ORIENTED_EDGE('',*,*,#7203,.F.);
#9396=ORIENTED_EDGE('',*,*,#7204,.T.);
#9397=ORIENTED_EDGE('',*,*,#7201,.T.);
#9398=ORIENTED_EDGE('',*,*,#7204,.F.);
#9399=ORIENTED_EDGE('',*,*,#7203,.T.);
#9400=ORIENTED_EDGE('',*,*,#7195,.F.);
#9401=ORIENTED_EDGE('',*,*,#7190,.T.);
#9402=ORIENTED_EDGE('',*,*,#7191,.T.);
#9403=ORIENTED_EDGE('',*,*,#7205,.T.);
#9404=ORIENTED_EDGE('',*,*,#7198,.F.);
#9405=ORIENTED_EDGE('',*,*,#7205,.F.);
#9406=ORIENTED_EDGE('',*,*,#7206,.T.);
#9407=ORIENTED_EDGE('',*,*,#7206,.F.);
#9408=ORIENTED_EDGE('',*,*,#7207,.T.);
#9409=ORIENTED_EDGE('',*,*,#7207,.F.);
#9410=ORIENTED_EDGE('',*,*,#7208,.T.);
#9411=ORIENTED_EDGE('',*,*,#7208,.F.);
#9412=ORIENTED_EDGE('',*,*,#7209,.T.);
#9413=ORIENTED_EDGE('',*,*,#7209,.F.);
#9414=ORIENTED_EDGE('',*,*,#7210,.T.);
#9415=ORIENTED_EDGE('',*,*,#7210,.F.);
#9416=ORIENTED_EDGE('',*,*,#7211,.T.);
#9417=ORIENTED_EDGE('',*,*,#7211,.F.);
#9418=ORIENTED_EDGE('',*,*,#7212,.T.);
#9419=ORIENTED_EDGE('',*,*,#7212,.F.);
#9420=ORIENTED_EDGE('',*,*,#7213,.F.);
#9421=ORIENTED_EDGE('',*,*,#7214,.F.);
#9422=ORIENTED_EDGE('',*,*,#7215,.F.);
#9423=ORIENTED_EDGE('',*,*,#7216,.F.);
#9424=ORIENTED_EDGE('',*,*,#7215,.T.);
#9425=ORIENTED_EDGE('',*,*,#7217,.F.);
#9426=ORIENTED_EDGE('',*,*,#7218,.T.);
#9427=ORIENTED_EDGE('',*,*,#7219,.F.);
#9428=ORIENTED_EDGE('',*,*,#7220,.T.);
#9429=ORIENTED_EDGE('',*,*,#7221,.F.);
#9430=ORIENTED_EDGE('',*,*,#7222,.T.);
#9431=ORIENTED_EDGE('',*,*,#7223,.F.);
#9432=ORIENTED_EDGE('',*,*,#7222,.F.);
#9433=ORIENTED_EDGE('',*,*,#7224,.F.);
#9434=ORIENTED_EDGE('',*,*,#7225,.T.);
#9435=ORIENTED_EDGE('',*,*,#7226,.F.);
#9436=ORIENTED_EDGE('',*,*,#7227,.T.);
#9437=ORIENTED_EDGE('',*,*,#7228,.F.);
#9438=ORIENTED_EDGE('',*,*,#7229,.T.);
#9439=ORIENTED_EDGE('',*,*,#7230,.F.);
#9440=ORIENTED_EDGE('',*,*,#7231,.T.);
#9441=ORIENTED_EDGE('',*,*,#7232,.F.);
#9442=ORIENTED_EDGE('',*,*,#7214,.T.);
#9443=ORIENTED_EDGE('',*,*,#7233,.T.);
#9444=ORIENTED_EDGE('',*,*,#7234,.T.);
#9445=ORIENTED_EDGE('',*,*,#7217,.T.);
#9446=ORIENTED_EDGE('',*,*,#7235,.F.);
#9447=ORIENTED_EDGE('',*,*,#7236,.F.);
#9448=ORIENTED_EDGE('',*,*,#7218,.F.);
#9449=ORIENTED_EDGE('',*,*,#7234,.F.);
#9450=ORIENTED_EDGE('',*,*,#7236,.T.);
#9451=ORIENTED_EDGE('',*,*,#7237,.T.);
#9452=ORIENTED_EDGE('',*,*,#7238,.T.);
#9453=ORIENTED_EDGE('',*,*,#7219,.T.);
#9454=ORIENTED_EDGE('',*,*,#7239,.F.);
#9455=ORIENTED_EDGE('',*,*,#7240,.F.);
#9456=ORIENTED_EDGE('',*,*,#7220,.F.);
#9457=ORIENTED_EDGE('',*,*,#7238,.F.);
#9458=ORIENTED_EDGE('',*,*,#7240,.T.);
#9459=ORIENTED_EDGE('',*,*,#7241,.T.);
#9460=ORIENTED_EDGE('',*,*,#7242,.T.);
#9461=ORIENTED_EDGE('',*,*,#7243,.T.);
#9462=ORIENTED_EDGE('',*,*,#7224,.T.);
#9463=ORIENTED_EDGE('',*,*,#7221,.T.);
#9464=ORIENTED_EDGE('',*,*,#7244,.F.);
#9465=ORIENTED_EDGE('',*,*,#7245,.F.);
#9466=ORIENTED_EDGE('',*,*,#7225,.F.);
#9467=ORIENTED_EDGE('',*,*,#7243,.F.);
#9468=ORIENTED_EDGE('',*,*,#7245,.T.);
#9469=ORIENTED_EDGE('',*,*,#7246,.T.);
#9470=ORIENTED_EDGE('',*,*,#7247,.T.);
#9471=ORIENTED_EDGE('',*,*,#7226,.T.);
#9472=ORIENTED_EDGE('',*,*,#7248,.F.);
#9473=ORIENTED_EDGE('',*,*,#7249,.F.);
#9474=ORIENTED_EDGE('',*,*,#7227,.F.);
#9475=ORIENTED_EDGE('',*,*,#7247,.F.);
#9476=ORIENTED_EDGE('',*,*,#7249,.T.);
#9477=ORIENTED_EDGE('',*,*,#7250,.T.);
#9478=ORIENTED_EDGE('',*,*,#7251,.T.);
#9479=ORIENTED_EDGE('',*,*,#7228,.T.);
#9480=ORIENTED_EDGE('',*,*,#7229,.F.);
#9481=ORIENTED_EDGE('',*,*,#7251,.F.);
#9482=ORIENTED_EDGE('',*,*,#7252,.F.);
#9483=ORIENTED_EDGE('',*,*,#7253,.F.);
#9484=ORIENTED_EDGE('',*,*,#7254,.F.);
#9485=ORIENTED_EDGE('',*,*,#7255,.T.);
#9486=ORIENTED_EDGE('',*,*,#7241,.F.);
#9487=ORIENTED_EDGE('',*,*,#7239,.T.);
#9488=ORIENTED_EDGE('',*,*,#7237,.F.);
#9489=ORIENTED_EDGE('',*,*,#7235,.T.);
#9490=ORIENTED_EDGE('',*,*,#7233,.F.);
#9491=ORIENTED_EDGE('',*,*,#7213,.T.);
#9492=ORIENTED_EDGE('',*,*,#7256,.F.);
#9493=ORIENTED_EDGE('',*,*,#7257,.T.);
#9494=ORIENTED_EDGE('',*,*,#7258,.F.);
#9495=ORIENTED_EDGE('',*,*,#7252,.T.);
#9496=ORIENTED_EDGE('',*,*,#7250,.F.);
#9497=ORIENTED_EDGE('',*,*,#7248,.T.);
#9498=ORIENTED_EDGE('',*,*,#7246,.F.);
#9499=ORIENTED_EDGE('',*,*,#7244,.T.);
#9500=ORIENTED_EDGE('',*,*,#7242,.F.);
#9501=ORIENTED_EDGE('',*,*,#7255,.F.);
#9502=ORIENTED_EDGE('',*,*,#7216,.T.);
#9503=ORIENTED_EDGE('',*,*,#7232,.T.);
#9504=ORIENTED_EDGE('',*,*,#7259,.T.);
#9505=ORIENTED_EDGE('',*,*,#7256,.T.);
#9506=ORIENTED_EDGE('',*,*,#7231,.F.);
#9507=ORIENTED_EDGE('',*,*,#7260,.F.);
#9508=ORIENTED_EDGE('',*,*,#7257,.F.);
#9509=ORIENTED_EDGE('',*,*,#7259,.F.);
#9510=ORIENTED_EDGE('',*,*,#7223,.T.);
#9511=ORIENTED_EDGE('',*,*,#7254,.T.);
#9512=ORIENTED_EDGE('',*,*,#7253,.T.);
#9513=ORIENTED_EDGE('',*,*,#7258,.T.);
#9514=ORIENTED_EDGE('',*,*,#7260,.T.);
#9515=ORIENTED_EDGE('',*,*,#7230,.T.);
#9516=ORIENTED_EDGE('',*,*,#7261,.F.);
#9517=ORIENTED_EDGE('',*,*,#7262,.T.);
#9518=ORIENTED_EDGE('',*,*,#7263,.F.);
#9519=ORIENTED_EDGE('',*,*,#7264,.T.);
#9520=ORIENTED_EDGE('',*,*,#7261,.T.);
#9521=ORIENTED_EDGE('',*,*,#7264,.F.);
#9522=ORIENTED_EDGE('',*,*,#7263,.T.);
#9523=ORIENTED_EDGE('',*,*,#7265,.F.);
#9524=ORIENTED_EDGE('',*,*,#7265,.T.);
#9525=ORIENTED_EDGE('',*,*,#7266,.T.);
#9526=ORIENTED_EDGE('',*,*,#7262,.F.);
#9527=ORIENTED_EDGE('',*,*,#7266,.F.);
#9528=ORIENTED_EDGE('',*,*,#7267,.F.);
#9529=ORIENTED_EDGE('',*,*,#7268,.T.);
#9530=ORIENTED_EDGE('',*,*,#7269,.F.);
#9531=ORIENTED_EDGE('',*,*,#7270,.T.);
#9532=ORIENTED_EDGE('',*,*,#7267,.T.);
#9533=ORIENTED_EDGE('',*,*,#7270,.F.);
#9534=ORIENTED_EDGE('',*,*,#7269,.T.);
#9535=ORIENTED_EDGE('',*,*,#7271,.F.);
#9536=ORIENTED_EDGE('',*,*,#7271,.T.);
#9537=ORIENTED_EDGE('',*,*,#7272,.T.);
#9538=ORIENTED_EDGE('',*,*,#7268,.F.);
#9539=ORIENTED_EDGE('',*,*,#7272,.F.);
#9540=ORIENTED_EDGE('',*,*,#7273,.T.);
#9541=ORIENTED_EDGE('',*,*,#7274,.T.);
#9542=ORIENTED_EDGE('',*,*,#7275,.T.);
#9543=ORIENTED_EDGE('',*,*,#7276,.F.);
#9544=ORIENTED_EDGE('',*,*,#7277,.T.);
#9545=ORIENTED_EDGE('',*,*,#7278,.T.);
#9546=ORIENTED_EDGE('',*,*,#7279,.T.);
#9547=ORIENTED_EDGE('',*,*,#7274,.F.);
#9548=ORIENTED_EDGE('',*,*,#7280,.T.);
#9549=ORIENTED_EDGE('',*,*,#7281,.T.);
#9550=ORIENTED_EDGE('',*,*,#7282,.T.);
#9551=ORIENTED_EDGE('',*,*,#7278,.F.);
#9552=ORIENTED_EDGE('',*,*,#7283,.T.);
#9553=ORIENTED_EDGE('',*,*,#7284,.T.);
#9554=ORIENTED_EDGE('',*,*,#7285,.T.);
#9555=ORIENTED_EDGE('',*,*,#7281,.F.);
#9556=ORIENTED_EDGE('',*,*,#7286,.T.);
#9557=ORIENTED_EDGE('',*,*,#7287,.T.);
#9558=ORIENTED_EDGE('',*,*,#7288,.T.);
#9559=ORIENTED_EDGE('',*,*,#7284,.F.);
#9560=ORIENTED_EDGE('',*,*,#7289,.T.);
#9561=ORIENTED_EDGE('',*,*,#7276,.T.);
#9562=ORIENTED_EDGE('',*,*,#7290,.T.);
#9563=ORIENTED_EDGE('',*,*,#7287,.F.);
#9564=ORIENTED_EDGE('',*,*,#7289,.F.);
#9565=ORIENTED_EDGE('',*,*,#7286,.F.);
#9566=ORIENTED_EDGE('',*,*,#7283,.F.);
#9567=ORIENTED_EDGE('',*,*,#7280,.F.);
#9568=ORIENTED_EDGE('',*,*,#7277,.F.);
#9569=ORIENTED_EDGE('',*,*,#7273,.F.);
#9570=ORIENTED_EDGE('',*,*,#7290,.F.);
#9571=ORIENTED_EDGE('',*,*,#7275,.F.);
#9572=ORIENTED_EDGE('',*,*,#7279,.F.);
#9573=ORIENTED_EDGE('',*,*,#7282,.F.);
#9574=ORIENTED_EDGE('',*,*,#7285,.F.);
#9575=ORIENTED_EDGE('',*,*,#7288,.F.);
#9576=ORIENTED_EDGE('',*,*,#7291,.F.);
#9577=ORIENTED_EDGE('',*,*,#7292,.F.);
#9578=ORIENTED_EDGE('',*,*,#7293,.F.);
#9579=ORIENTED_EDGE('',*,*,#7294,.T.);
#9580=ORIENTED_EDGE('',*,*,#7292,.T.);
#9581=ORIENTED_EDGE('',*,*,#7294,.F.);
#9582=ORIENTED_EDGE('',*,*,#7295,.F.);
#9583=ORIENTED_EDGE('',*,*,#7296,.T.);
#9584=ORIENTED_EDGE('',*,*,#7293,.T.);
#9585=ORIENTED_EDGE('',*,*,#7296,.F.);
#9586=ORIENTED_EDGE('',*,*,#7297,.F.);
#9587=ORIENTED_EDGE('',*,*,#7298,.T.);
#9588=ORIENTED_EDGE('',*,*,#7295,.T.);
#9589=ORIENTED_EDGE('',*,*,#7298,.F.);
#9590=ORIENTED_EDGE('',*,*,#7297,.T.);
#9591=ORIENTED_EDGE('',*,*,#7299,.F.);
#9592=ORIENTED_EDGE('',*,*,#7300,.F.);
#9593=ORIENTED_EDGE('',*,*,#7301,.T.);
#9594=ORIENTED_EDGE('',*,*,#7299,.T.);
#9595=ORIENTED_EDGE('',*,*,#7301,.F.);
#9596=ORIENTED_EDGE('',*,*,#7291,.T.);
#9597=ORIENTED_EDGE('',*,*,#7302,.T.);
#9598=ORIENTED_EDGE('',*,*,#7300,.T.);
#9599=ORIENTED_EDGE('',*,*,#7302,.F.);
#9600=ORIENTED_EDGE('',*,*,#7303,.F.);
#9601=ORIENTED_EDGE('',*,*,#7304,.T.);
#9602=ORIENTED_EDGE('',*,*,#7305,.T.);
#9603=ORIENTED_EDGE('',*,*,#7304,.F.);
#9604=ORIENTED_EDGE('',*,*,#7305,.F.);
#9605=ORIENTED_EDGE('',*,*,#7306,.F.);
#9606=ORIENTED_EDGE('',*,*,#7307,.F.);
#9607=ORIENTED_EDGE('',*,*,#7308,.F.);
#9608=ORIENTED_EDGE('',*,*,#7309,.T.);
#9609=ORIENTED_EDGE('',*,*,#7310,.F.);
#9610=ORIENTED_EDGE('',*,*,#7311,.T.);
#9611=ORIENTED_EDGE('',*,*,#7312,.F.);
#9612=ORIENTED_EDGE('',*,*,#7313,.F.);
#9613=ORIENTED_EDGE('',*,*,#7314,.F.);
#9614=ORIENTED_EDGE('',*,*,#7309,.F.);
#9615=ORIENTED_EDGE('',*,*,#7315,.F.);
#9616=ORIENTED_EDGE('',*,*,#7316,.T.);
#9617=ORIENTED_EDGE('',*,*,#7317,.F.);
#9618=ORIENTED_EDGE('',*,*,#7311,.F.);
#9619=ORIENTED_EDGE('',*,*,#7318,.F.);
#9620=ORIENTED_EDGE('',*,*,#7319,.F.);
#9621=ORIENTED_EDGE('',*,*,#7313,.T.);
#9622=ORIENTED_EDGE('',*,*,#7320,.F.);
#9623=ORIENTED_EDGE('',*,*,#7321,.F.);
#9624=ORIENTED_EDGE('',*,*,#7322,.F.);
#9625=ORIENTED_EDGE('',*,*,#7307,.T.);
#9626=ORIENTED_EDGE('',*,*,#7323,.F.);
#9627=ORIENTED_EDGE('',*,*,#7324,.F.);
#9628=ORIENTED_EDGE('',*,*,#7321,.T.);
#9629=ORIENTED_EDGE('',*,*,#7325,.F.);
#9630=ORIENTED_EDGE('',*,*,#7326,.F.);
#9631=ORIENTED_EDGE('',*,*,#7327,.F.);
#9632=ORIENTED_EDGE('',*,*,#7326,.T.);
#9633=ORIENTED_EDGE('',*,*,#7328,.F.);
#9634=ORIENTED_EDGE('',*,*,#7329,.F.);
#9635=ORIENTED_EDGE('',*,*,#7330,.F.);
#9636=ORIENTED_EDGE('',*,*,#7329,.T.);
#9637=ORIENTED_EDGE('',*,*,#7331,.F.);
#9638=ORIENTED_EDGE('',*,*,#7332,.F.);
#9639=ORIENTED_EDGE('',*,*,#7333,.F.);
#9640=ORIENTED_EDGE('',*,*,#7332,.T.);
#9641=ORIENTED_EDGE('',*,*,#7334,.F.);
#9642=ORIENTED_EDGE('',*,*,#7335,.F.);
#9643=ORIENTED_EDGE('',*,*,#7336,.F.);
#9644=ORIENTED_EDGE('',*,*,#7335,.T.);
#9645=ORIENTED_EDGE('',*,*,#7337,.F.);
#9646=ORIENTED_EDGE('',*,*,#7338,.F.);
#9647=ORIENTED_EDGE('',*,*,#7339,.F.);
#9648=ORIENTED_EDGE('',*,*,#7338,.T.);
#9649=ORIENTED_EDGE('',*,*,#7340,.F.);
#9650=ORIENTED_EDGE('',*,*,#7341,.F.);
#9651=ORIENTED_EDGE('',*,*,#7342,.F.);
#9652=ORIENTED_EDGE('',*,*,#7341,.T.);
#9653=ORIENTED_EDGE('',*,*,#7343,.F.);
#9654=ORIENTED_EDGE('',*,*,#7344,.F.);
#9655=ORIENTED_EDGE('',*,*,#7345,.F.);
#9656=ORIENTED_EDGE('',*,*,#7344,.T.);
#9657=ORIENTED_EDGE('',*,*,#7346,.F.);
#9658=ORIENTED_EDGE('',*,*,#7347,.F.);
#9659=ORIENTED_EDGE('',*,*,#7348,.F.);
#9660=ORIENTED_EDGE('',*,*,#7347,.T.);
#9661=ORIENTED_EDGE('',*,*,#7349,.F.);
#9662=ORIENTED_EDGE('',*,*,#7350,.F.);
#9663=ORIENTED_EDGE('',*,*,#7351,.F.);
#9664=ORIENTED_EDGE('',*,*,#7350,.T.);
#9665=ORIENTED_EDGE('',*,*,#7352,.F.);
#9666=ORIENTED_EDGE('',*,*,#7353,.F.);
#9667=ORIENTED_EDGE('',*,*,#7354,.F.);
#9668=ORIENTED_EDGE('',*,*,#7353,.T.);
#9669=ORIENTED_EDGE('',*,*,#7355,.F.);
#9670=ORIENTED_EDGE('',*,*,#7356,.F.);
#9671=ORIENTED_EDGE('',*,*,#7357,.F.);
#9672=ORIENTED_EDGE('',*,*,#7356,.T.);
#9673=ORIENTED_EDGE('',*,*,#7358,.F.);
#9674=ORIENTED_EDGE('',*,*,#7359,.F.);
#9675=ORIENTED_EDGE('',*,*,#7360,.F.);
#9676=ORIENTED_EDGE('',*,*,#7359,.T.);
#9677=ORIENTED_EDGE('',*,*,#7361,.F.);
#9678=ORIENTED_EDGE('',*,*,#7362,.F.);
#9679=ORIENTED_EDGE('',*,*,#7363,.F.);
#9680=ORIENTED_EDGE('',*,*,#7362,.T.);
#9681=ORIENTED_EDGE('',*,*,#7364,.F.);
#9682=ORIENTED_EDGE('',*,*,#7365,.F.);
#9683=ORIENTED_EDGE('',*,*,#7366,.F.);
#9684=ORIENTED_EDGE('',*,*,#7365,.T.);
#9685=ORIENTED_EDGE('',*,*,#7367,.F.);
#9686=ORIENTED_EDGE('',*,*,#7368,.F.);
#9687=ORIENTED_EDGE('',*,*,#7369,.F.);
#9688=ORIENTED_EDGE('',*,*,#7368,.T.);
#9689=ORIENTED_EDGE('',*,*,#7370,.F.);
#9690=ORIENTED_EDGE('',*,*,#7371,.F.);
#9691=ORIENTED_EDGE('',*,*,#7372,.F.);
#9692=ORIENTED_EDGE('',*,*,#7371,.T.);
#9693=ORIENTED_EDGE('',*,*,#7373,.F.);
#9694=ORIENTED_EDGE('',*,*,#7374,.F.);
#9695=ORIENTED_EDGE('',*,*,#7375,.F.);
#9696=ORIENTED_EDGE('',*,*,#7374,.T.);
#9697=ORIENTED_EDGE('',*,*,#7376,.F.);
#9698=ORIENTED_EDGE('',*,*,#7377,.F.);
#9699=ORIENTED_EDGE('',*,*,#7378,.F.);
#9700=ORIENTED_EDGE('',*,*,#7377,.T.);
#9701=ORIENTED_EDGE('',*,*,#7379,.F.);
#9702=ORIENTED_EDGE('',*,*,#7380,.F.);
#9703=ORIENTED_EDGE('',*,*,#7381,.F.);
#9704=ORIENTED_EDGE('',*,*,#7380,.T.);
#9705=ORIENTED_EDGE('',*,*,#7382,.F.);
#9706=ORIENTED_EDGE('',*,*,#7383,.F.);
#9707=ORIENTED_EDGE('',*,*,#7384,.F.);
#9708=ORIENTED_EDGE('',*,*,#7383,.T.);
#9709=ORIENTED_EDGE('',*,*,#7385,.F.);
#9710=ORIENTED_EDGE('',*,*,#7386,.F.);
#9711=ORIENTED_EDGE('',*,*,#7387,.F.);
#9712=ORIENTED_EDGE('',*,*,#7386,.T.);
#9713=ORIENTED_EDGE('',*,*,#7388,.F.);
#9714=ORIENTED_EDGE('',*,*,#7389,.F.);
#9715=ORIENTED_EDGE('',*,*,#7390,.F.);
#9716=ORIENTED_EDGE('',*,*,#7389,.T.);
#9717=ORIENTED_EDGE('',*,*,#7391,.F.);
#9718=ORIENTED_EDGE('',*,*,#7392,.F.);
#9719=ORIENTED_EDGE('',*,*,#7393,.F.);
#9720=ORIENTED_EDGE('',*,*,#7392,.T.);
#9721=ORIENTED_EDGE('',*,*,#7394,.F.);
#9722=ORIENTED_EDGE('',*,*,#7395,.F.);
#9723=ORIENTED_EDGE('',*,*,#7396,.F.);
#9724=ORIENTED_EDGE('',*,*,#7395,.T.);
#9725=ORIENTED_EDGE('',*,*,#7397,.F.);
#9726=ORIENTED_EDGE('',*,*,#7398,.F.);
#9727=ORIENTED_EDGE('',*,*,#7399,.F.);
#9728=ORIENTED_EDGE('',*,*,#7398,.T.);
#9729=ORIENTED_EDGE('',*,*,#7400,.F.);
#9730=ORIENTED_EDGE('',*,*,#7401,.F.);
#9731=ORIENTED_EDGE('',*,*,#7402,.F.);
#9732=ORIENTED_EDGE('',*,*,#7401,.T.);
#9733=ORIENTED_EDGE('',*,*,#7403,.F.);
#9734=ORIENTED_EDGE('',*,*,#7404,.F.);
#9735=ORIENTED_EDGE('',*,*,#7405,.F.);
#9736=ORIENTED_EDGE('',*,*,#7404,.T.);
#9737=ORIENTED_EDGE('',*,*,#7406,.F.);
#9738=ORIENTED_EDGE('',*,*,#7407,.F.);
#9739=ORIENTED_EDGE('',*,*,#7408,.F.);
#9740=ORIENTED_EDGE('',*,*,#7407,.T.);
#9741=ORIENTED_EDGE('',*,*,#7409,.F.);
#9742=ORIENTED_EDGE('',*,*,#7410,.F.);
#9743=ORIENTED_EDGE('',*,*,#7411,.F.);
#9744=ORIENTED_EDGE('',*,*,#7410,.T.);
#9745=ORIENTED_EDGE('',*,*,#7412,.F.);
#9746=ORIENTED_EDGE('',*,*,#7413,.F.);
#9747=ORIENTED_EDGE('',*,*,#7414,.F.);
#9748=ORIENTED_EDGE('',*,*,#7413,.T.);
#9749=ORIENTED_EDGE('',*,*,#7415,.F.);
#9750=ORIENTED_EDGE('',*,*,#7416,.F.);
#9751=ORIENTED_EDGE('',*,*,#7417,.F.);
#9752=ORIENTED_EDGE('',*,*,#7416,.T.);
#9753=ORIENTED_EDGE('',*,*,#7418,.F.);
#9754=ORIENTED_EDGE('',*,*,#7419,.F.);
#9755=ORIENTED_EDGE('',*,*,#7420,.F.);
#9756=ORIENTED_EDGE('',*,*,#7419,.T.);
#9757=ORIENTED_EDGE('',*,*,#7421,.F.);
#9758=ORIENTED_EDGE('',*,*,#7422,.F.);
#9759=ORIENTED_EDGE('',*,*,#7423,.F.);
#9760=ORIENTED_EDGE('',*,*,#7422,.T.);
#9761=ORIENTED_EDGE('',*,*,#7424,.F.);
#9762=ORIENTED_EDGE('',*,*,#7425,.F.);
#9763=ORIENTED_EDGE('',*,*,#7426,.F.);
#9764=ORIENTED_EDGE('',*,*,#7425,.T.);
#9765=ORIENTED_EDGE('',*,*,#7427,.F.);
#9766=ORIENTED_EDGE('',*,*,#7428,.F.);
#9767=ORIENTED_EDGE('',*,*,#7429,.F.);
#9768=ORIENTED_EDGE('',*,*,#7428,.T.);
#9769=ORIENTED_EDGE('',*,*,#7430,.F.);
#9770=ORIENTED_EDGE('',*,*,#7431,.F.);
#9771=ORIENTED_EDGE('',*,*,#7432,.F.);
#9772=ORIENTED_EDGE('',*,*,#7431,.T.);
#9773=ORIENTED_EDGE('',*,*,#7433,.F.);
#9774=ORIENTED_EDGE('',*,*,#7434,.F.);
#9775=ORIENTED_EDGE('',*,*,#7435,.F.);
#9776=ORIENTED_EDGE('',*,*,#7434,.T.);
#9777=ORIENTED_EDGE('',*,*,#7436,.F.);
#9778=ORIENTED_EDGE('',*,*,#7437,.F.);
#9779=ORIENTED_EDGE('',*,*,#7438,.F.);
#9780=ORIENTED_EDGE('',*,*,#7437,.T.);
#9781=ORIENTED_EDGE('',*,*,#7439,.F.);
#9782=ORIENTED_EDGE('',*,*,#7440,.F.);
#9783=ORIENTED_EDGE('',*,*,#7441,.F.);
#9784=ORIENTED_EDGE('',*,*,#7440,.T.);
#9785=ORIENTED_EDGE('',*,*,#7442,.F.);
#9786=ORIENTED_EDGE('',*,*,#7443,.F.);
#9787=ORIENTED_EDGE('',*,*,#7444,.F.);
#9788=ORIENTED_EDGE('',*,*,#7443,.T.);
#9789=ORIENTED_EDGE('',*,*,#7445,.F.);
#9790=ORIENTED_EDGE('',*,*,#7446,.F.);
#9791=ORIENTED_EDGE('',*,*,#7447,.F.);
#9792=ORIENTED_EDGE('',*,*,#7446,.T.);
#9793=ORIENTED_EDGE('',*,*,#7448,.F.);
#9794=ORIENTED_EDGE('',*,*,#7449,.F.);
#9795=ORIENTED_EDGE('',*,*,#7450,.F.);
#9796=ORIENTED_EDGE('',*,*,#7449,.T.);
#9797=ORIENTED_EDGE('',*,*,#7451,.F.);
#9798=ORIENTED_EDGE('',*,*,#7452,.F.);
#9799=ORIENTED_EDGE('',*,*,#7453,.F.);
#9800=ORIENTED_EDGE('',*,*,#7452,.T.);
#9801=ORIENTED_EDGE('',*,*,#7454,.F.);
#9802=ORIENTED_EDGE('',*,*,#7455,.F.);
#9803=ORIENTED_EDGE('',*,*,#7456,.F.);
#9804=ORIENTED_EDGE('',*,*,#7455,.T.);
#9805=ORIENTED_EDGE('',*,*,#7457,.F.);
#9806=ORIENTED_EDGE('',*,*,#7458,.F.);
#9807=ORIENTED_EDGE('',*,*,#7459,.F.);
#9808=ORIENTED_EDGE('',*,*,#7458,.T.);
#9809=ORIENTED_EDGE('',*,*,#7460,.F.);
#9810=ORIENTED_EDGE('',*,*,#7461,.F.);
#9811=ORIENTED_EDGE('',*,*,#7462,.F.);
#9812=ORIENTED_EDGE('',*,*,#7461,.T.);
#9813=ORIENTED_EDGE('',*,*,#7463,.F.);
#9814=ORIENTED_EDGE('',*,*,#7464,.F.);
#9815=ORIENTED_EDGE('',*,*,#7465,.F.);
#9816=ORIENTED_EDGE('',*,*,#7464,.T.);
#9817=ORIENTED_EDGE('',*,*,#7466,.F.);
#9818=ORIENTED_EDGE('',*,*,#7467,.F.);
#9819=ORIENTED_EDGE('',*,*,#7468,.F.);
#9820=ORIENTED_EDGE('',*,*,#7467,.T.);
#9821=ORIENTED_EDGE('',*,*,#7469,.F.);
#9822=ORIENTED_EDGE('',*,*,#7470,.F.);
#9823=ORIENTED_EDGE('',*,*,#7471,.F.);
#9824=ORIENTED_EDGE('',*,*,#7470,.T.);
#9825=ORIENTED_EDGE('',*,*,#7472,.F.);
#9826=ORIENTED_EDGE('',*,*,#7473,.F.);
#9827=ORIENTED_EDGE('',*,*,#7474,.F.);
#9828=ORIENTED_EDGE('',*,*,#7473,.T.);
#9829=ORIENTED_EDGE('',*,*,#7475,.F.);
#9830=ORIENTED_EDGE('',*,*,#7476,.F.);
#9831=ORIENTED_EDGE('',*,*,#7477,.F.);
#9832=ORIENTED_EDGE('',*,*,#7476,.T.);
#9833=ORIENTED_EDGE('',*,*,#7478,.F.);
#9834=ORIENTED_EDGE('',*,*,#7479,.F.);
#9835=ORIENTED_EDGE('',*,*,#7480,.F.);
#9836=ORIENTED_EDGE('',*,*,#7479,.T.);
#9837=ORIENTED_EDGE('',*,*,#7481,.F.);
#9838=ORIENTED_EDGE('',*,*,#7482,.F.);
#9839=ORIENTED_EDGE('',*,*,#7483,.F.);
#9840=ORIENTED_EDGE('',*,*,#7482,.T.);
#9841=ORIENTED_EDGE('',*,*,#7484,.F.);
#9842=ORIENTED_EDGE('',*,*,#7485,.F.);
#9843=ORIENTED_EDGE('',*,*,#7486,.F.);
#9844=ORIENTED_EDGE('',*,*,#7485,.T.);
#9845=ORIENTED_EDGE('',*,*,#7487,.F.);
#9846=ORIENTED_EDGE('',*,*,#7488,.F.);
#9847=ORIENTED_EDGE('',*,*,#7489,.F.);
#9848=ORIENTED_EDGE('',*,*,#7488,.T.);
#9849=ORIENTED_EDGE('',*,*,#7490,.F.);
#9850=ORIENTED_EDGE('',*,*,#7491,.F.);
#9851=ORIENTED_EDGE('',*,*,#7492,.F.);
#9852=ORIENTED_EDGE('',*,*,#7491,.T.);
#9853=ORIENTED_EDGE('',*,*,#7493,.F.);
#9854=ORIENTED_EDGE('',*,*,#7494,.F.);
#9855=ORIENTED_EDGE('',*,*,#7495,.F.);
#9856=ORIENTED_EDGE('',*,*,#7494,.T.);
#9857=ORIENTED_EDGE('',*,*,#7496,.F.);
#9858=ORIENTED_EDGE('',*,*,#7497,.F.);
#9859=ORIENTED_EDGE('',*,*,#7498,.F.);
#9860=ORIENTED_EDGE('',*,*,#7497,.T.);
#9861=ORIENTED_EDGE('',*,*,#7499,.F.);
#9862=ORIENTED_EDGE('',*,*,#7500,.F.);
#9863=ORIENTED_EDGE('',*,*,#7501,.F.);
#9864=ORIENTED_EDGE('',*,*,#7500,.T.);
#9865=ORIENTED_EDGE('',*,*,#7502,.F.);
#9866=ORIENTED_EDGE('',*,*,#7503,.F.);
#9867=ORIENTED_EDGE('',*,*,#7504,.F.);
#9868=ORIENTED_EDGE('',*,*,#7503,.T.);
#9869=ORIENTED_EDGE('',*,*,#7505,.F.);
#9870=ORIENTED_EDGE('',*,*,#7506,.F.);
#9871=ORIENTED_EDGE('',*,*,#7507,.F.);
#9872=ORIENTED_EDGE('',*,*,#7506,.T.);
#9873=ORIENTED_EDGE('',*,*,#7508,.F.);
#9874=ORIENTED_EDGE('',*,*,#7509,.F.);
#9875=ORIENTED_EDGE('',*,*,#7510,.F.);
#9876=ORIENTED_EDGE('',*,*,#7509,.T.);
#9877=ORIENTED_EDGE('',*,*,#7511,.F.);
#9878=ORIENTED_EDGE('',*,*,#7512,.F.);
#9879=ORIENTED_EDGE('',*,*,#7513,.F.);
#9880=ORIENTED_EDGE('',*,*,#7512,.T.);
#9881=ORIENTED_EDGE('',*,*,#7514,.F.);
#9882=ORIENTED_EDGE('',*,*,#7515,.F.);
#9883=ORIENTED_EDGE('',*,*,#7516,.F.);
#9884=ORIENTED_EDGE('',*,*,#7515,.T.);
#9885=ORIENTED_EDGE('',*,*,#7517,.F.);
#9886=ORIENTED_EDGE('',*,*,#7518,.F.);
#9887=ORIENTED_EDGE('',*,*,#7519,.F.);
#9888=ORIENTED_EDGE('',*,*,#7518,.T.);
#9889=ORIENTED_EDGE('',*,*,#7520,.F.);
#9890=ORIENTED_EDGE('',*,*,#7521,.F.);
#9891=ORIENTED_EDGE('',*,*,#7522,.F.);
#9892=ORIENTED_EDGE('',*,*,#7521,.T.);
#9893=ORIENTED_EDGE('',*,*,#7523,.F.);
#9894=ORIENTED_EDGE('',*,*,#7524,.F.);
#9895=ORIENTED_EDGE('',*,*,#7525,.F.);
#9896=ORIENTED_EDGE('',*,*,#7524,.T.);
#9897=ORIENTED_EDGE('',*,*,#7526,.F.);
#9898=ORIENTED_EDGE('',*,*,#7527,.F.);
#9899=ORIENTED_EDGE('',*,*,#7528,.F.);
#9900=ORIENTED_EDGE('',*,*,#7527,.T.);
#9901=ORIENTED_EDGE('',*,*,#7529,.F.);
#9902=ORIENTED_EDGE('',*,*,#7530,.F.);
#9903=ORIENTED_EDGE('',*,*,#7531,.F.);
#9904=ORIENTED_EDGE('',*,*,#7530,.T.);
#9905=ORIENTED_EDGE('',*,*,#7532,.F.);
#9906=ORIENTED_EDGE('',*,*,#7533,.F.);
#9907=ORIENTED_EDGE('',*,*,#7534,.F.);
#9908=ORIENTED_EDGE('',*,*,#7533,.T.);
#9909=ORIENTED_EDGE('',*,*,#7535,.F.);
#9910=ORIENTED_EDGE('',*,*,#7536,.F.);
#9911=ORIENTED_EDGE('',*,*,#7537,.F.);
#9912=ORIENTED_EDGE('',*,*,#7536,.T.);
#9913=ORIENTED_EDGE('',*,*,#7538,.F.);
#9914=ORIENTED_EDGE('',*,*,#7539,.F.);
#9915=ORIENTED_EDGE('',*,*,#7540,.F.);
#9916=ORIENTED_EDGE('',*,*,#7539,.T.);
#9917=ORIENTED_EDGE('',*,*,#7541,.F.);
#9918=ORIENTED_EDGE('',*,*,#7542,.F.);
#9919=ORIENTED_EDGE('',*,*,#7543,.F.);
#9920=ORIENTED_EDGE('',*,*,#7542,.T.);
#9921=ORIENTED_EDGE('',*,*,#7544,.F.);
#9922=ORIENTED_EDGE('',*,*,#7545,.F.);
#9923=ORIENTED_EDGE('',*,*,#7546,.F.);
#9924=ORIENTED_EDGE('',*,*,#7545,.T.);
#9925=ORIENTED_EDGE('',*,*,#7547,.F.);
#9926=ORIENTED_EDGE('',*,*,#7548,.F.);
#9927=ORIENTED_EDGE('',*,*,#7549,.F.);
#9928=ORIENTED_EDGE('',*,*,#7548,.T.);
#9929=ORIENTED_EDGE('',*,*,#7550,.F.);
#9930=ORIENTED_EDGE('',*,*,#7551,.F.);
#9931=ORIENTED_EDGE('',*,*,#7552,.F.);
#9932=ORIENTED_EDGE('',*,*,#7551,.T.);
#9933=ORIENTED_EDGE('',*,*,#7553,.F.);
#9934=ORIENTED_EDGE('',*,*,#7554,.F.);
#9935=ORIENTED_EDGE('',*,*,#7555,.F.);
#9936=ORIENTED_EDGE('',*,*,#7554,.T.);
#9937=ORIENTED_EDGE('',*,*,#7556,.F.);
#9938=ORIENTED_EDGE('',*,*,#7557,.F.);
#9939=ORIENTED_EDGE('',*,*,#7558,.F.);
#9940=ORIENTED_EDGE('',*,*,#7557,.T.);
#9941=ORIENTED_EDGE('',*,*,#7559,.F.);
#9942=ORIENTED_EDGE('',*,*,#7560,.F.);
#9943=ORIENTED_EDGE('',*,*,#7561,.F.);
#9944=ORIENTED_EDGE('',*,*,#7560,.T.);
#9945=ORIENTED_EDGE('',*,*,#7562,.F.);
#9946=ORIENTED_EDGE('',*,*,#7563,.F.);
#9947=ORIENTED_EDGE('',*,*,#7564,.F.);
#9948=ORIENTED_EDGE('',*,*,#7563,.T.);
#9949=ORIENTED_EDGE('',*,*,#7565,.F.);
#9950=ORIENTED_EDGE('',*,*,#7566,.F.);
#9951=ORIENTED_EDGE('',*,*,#7567,.F.);
#9952=ORIENTED_EDGE('',*,*,#7566,.T.);
#9953=ORIENTED_EDGE('',*,*,#7568,.F.);
#9954=ORIENTED_EDGE('',*,*,#7569,.F.);
#9955=ORIENTED_EDGE('',*,*,#7570,.F.);
#9956=ORIENTED_EDGE('',*,*,#7569,.T.);
#9957=ORIENTED_EDGE('',*,*,#7571,.F.);
#9958=ORIENTED_EDGE('',*,*,#7572,.F.);
#9959=ORIENTED_EDGE('',*,*,#7573,.F.);
#9960=ORIENTED_EDGE('',*,*,#7572,.T.);
#9961=ORIENTED_EDGE('',*,*,#7574,.F.);
#9962=ORIENTED_EDGE('',*,*,#7575,.F.);
#9963=ORIENTED_EDGE('',*,*,#7576,.F.);
#9964=ORIENTED_EDGE('',*,*,#7575,.T.);
#9965=ORIENTED_EDGE('',*,*,#7577,.F.);
#9966=ORIENTED_EDGE('',*,*,#7578,.F.);
#9967=ORIENTED_EDGE('',*,*,#7579,.F.);
#9968=ORIENTED_EDGE('',*,*,#7578,.T.);
#9969=ORIENTED_EDGE('',*,*,#7580,.F.);
#9970=ORIENTED_EDGE('',*,*,#7581,.F.);
#9971=ORIENTED_EDGE('',*,*,#7582,.F.);
#9972=ORIENTED_EDGE('',*,*,#7581,.T.);
#9973=ORIENTED_EDGE('',*,*,#7583,.F.);
#9974=ORIENTED_EDGE('',*,*,#7584,.F.);
#9975=ORIENTED_EDGE('',*,*,#7585,.F.);
#9976=ORIENTED_EDGE('',*,*,#7584,.T.);
#9977=ORIENTED_EDGE('',*,*,#7586,.F.);
#9978=ORIENTED_EDGE('',*,*,#7587,.F.);
#9979=ORIENTED_EDGE('',*,*,#7588,.F.);
#9980=ORIENTED_EDGE('',*,*,#7587,.T.);
#9981=ORIENTED_EDGE('',*,*,#7589,.F.);
#9982=ORIENTED_EDGE('',*,*,#7590,.F.);
#9983=ORIENTED_EDGE('',*,*,#7591,.F.);
#9984=ORIENTED_EDGE('',*,*,#7590,.T.);
#9985=ORIENTED_EDGE('',*,*,#7592,.F.);
#9986=ORIENTED_EDGE('',*,*,#7593,.F.);
#9987=ORIENTED_EDGE('',*,*,#7594,.F.);
#9988=ORIENTED_EDGE('',*,*,#7593,.T.);
#9989=ORIENTED_EDGE('',*,*,#7595,.F.);
#9990=ORIENTED_EDGE('',*,*,#7596,.F.);
#9991=ORIENTED_EDGE('',*,*,#7597,.F.);
#9992=ORIENTED_EDGE('',*,*,#7596,.T.);
#9993=ORIENTED_EDGE('',*,*,#7598,.F.);
#9994=ORIENTED_EDGE('',*,*,#7599,.F.);
#9995=ORIENTED_EDGE('',*,*,#7600,.F.);
#9996=ORIENTED_EDGE('',*,*,#7599,.T.);
#9997=ORIENTED_EDGE('',*,*,#7601,.F.);
#9998=ORIENTED_EDGE('',*,*,#7602,.F.);
#9999=ORIENTED_EDGE('',*,*,#7603,.F.);
#10000=ORIENTED_EDGE('',*,*,#7602,.T.);
#10001=ORIENTED_EDGE('',*,*,#7604,.F.);
#10002=ORIENTED_EDGE('',*,*,#7605,.F.);
#10003=ORIENTED_EDGE('',*,*,#7606,.F.);
#10004=ORIENTED_EDGE('',*,*,#7605,.T.);
#10005=ORIENTED_EDGE('',*,*,#7607,.F.);
#10006=ORIENTED_EDGE('',*,*,#7608,.F.);
#10007=ORIENTED_EDGE('',*,*,#7609,.F.);
#10008=ORIENTED_EDGE('',*,*,#7608,.T.);
#10009=ORIENTED_EDGE('',*,*,#7610,.F.);
#10010=ORIENTED_EDGE('',*,*,#7611,.F.);
#10011=ORIENTED_EDGE('',*,*,#7612,.F.);
#10012=ORIENTED_EDGE('',*,*,#7611,.T.);
#10013=ORIENTED_EDGE('',*,*,#7613,.F.);
#10014=ORIENTED_EDGE('',*,*,#7614,.F.);
#10015=ORIENTED_EDGE('',*,*,#7615,.F.);
#10016=ORIENTED_EDGE('',*,*,#7614,.T.);
#10017=ORIENTED_EDGE('',*,*,#7616,.F.);
#10018=ORIENTED_EDGE('',*,*,#7617,.F.);
#10019=ORIENTED_EDGE('',*,*,#7618,.F.);
#10020=ORIENTED_EDGE('',*,*,#7617,.T.);
#10021=ORIENTED_EDGE('',*,*,#7619,.F.);
#10022=ORIENTED_EDGE('',*,*,#7620,.F.);
#10023=ORIENTED_EDGE('',*,*,#7621,.F.);
#10024=ORIENTED_EDGE('',*,*,#7620,.T.);
#10025=ORIENTED_EDGE('',*,*,#7622,.F.);
#10026=ORIENTED_EDGE('',*,*,#7623,.F.);
#10027=ORIENTED_EDGE('',*,*,#7624,.F.);
#10028=ORIENTED_EDGE('',*,*,#7623,.T.);
#10029=ORIENTED_EDGE('',*,*,#7625,.F.);
#10030=ORIENTED_EDGE('',*,*,#7626,.F.);
#10031=ORIENTED_EDGE('',*,*,#7627,.F.);
#10032=ORIENTED_EDGE('',*,*,#7626,.T.);
#10033=ORIENTED_EDGE('',*,*,#7628,.F.);
#10034=ORIENTED_EDGE('',*,*,#7629,.F.);
#10035=ORIENTED_EDGE('',*,*,#7630,.F.);
#10036=ORIENTED_EDGE('',*,*,#7629,.T.);
#10037=ORIENTED_EDGE('',*,*,#7631,.F.);
#10038=ORIENTED_EDGE('',*,*,#7632,.F.);
#10039=ORIENTED_EDGE('',*,*,#7633,.F.);
#10040=ORIENTED_EDGE('',*,*,#7632,.T.);
#10041=ORIENTED_EDGE('',*,*,#7634,.F.);
#10042=ORIENTED_EDGE('',*,*,#7635,.F.);
#10043=ORIENTED_EDGE('',*,*,#7636,.F.);
#10044=ORIENTED_EDGE('',*,*,#7635,.T.);
#10045=ORIENTED_EDGE('',*,*,#7637,.F.);
#10046=ORIENTED_EDGE('',*,*,#7638,.F.);
#10047=ORIENTED_EDGE('',*,*,#7639,.F.);
#10048=ORIENTED_EDGE('',*,*,#7638,.T.);
#10049=ORIENTED_EDGE('',*,*,#7640,.F.);
#10050=ORIENTED_EDGE('',*,*,#7641,.F.);
#10051=ORIENTED_EDGE('',*,*,#7642,.F.);
#10052=ORIENTED_EDGE('',*,*,#7641,.T.);
#10053=ORIENTED_EDGE('',*,*,#7643,.F.);
#10054=ORIENTED_EDGE('',*,*,#7644,.F.);
#10055=ORIENTED_EDGE('',*,*,#7645,.F.);
#10056=ORIENTED_EDGE('',*,*,#7644,.T.);
#10057=ORIENTED_EDGE('',*,*,#7646,.F.);
#10058=ORIENTED_EDGE('',*,*,#7647,.F.);
#10059=ORIENTED_EDGE('',*,*,#7648,.F.);
#10060=ORIENTED_EDGE('',*,*,#7647,.T.);
#10061=ORIENTED_EDGE('',*,*,#7649,.F.);
#10062=ORIENTED_EDGE('',*,*,#7650,.F.);
#10063=ORIENTED_EDGE('',*,*,#7651,.F.);
#10064=ORIENTED_EDGE('',*,*,#7650,.T.);
#10065=ORIENTED_EDGE('',*,*,#7652,.F.);
#10066=ORIENTED_EDGE('',*,*,#7653,.F.);
#10067=ORIENTED_EDGE('',*,*,#7654,.F.);
#10068=ORIENTED_EDGE('',*,*,#7653,.T.);
#10069=ORIENTED_EDGE('',*,*,#7655,.F.);
#10070=ORIENTED_EDGE('',*,*,#7656,.F.);
#10071=ORIENTED_EDGE('',*,*,#7657,.F.);
#10072=ORIENTED_EDGE('',*,*,#7656,.T.);
#10073=ORIENTED_EDGE('',*,*,#7658,.F.);
#10074=ORIENTED_EDGE('',*,*,#7659,.F.);
#10075=ORIENTED_EDGE('',*,*,#7660,.F.);
#10076=ORIENTED_EDGE('',*,*,#7659,.T.);
#10077=ORIENTED_EDGE('',*,*,#7661,.F.);
#10078=ORIENTED_EDGE('',*,*,#7662,.F.);
#10079=ORIENTED_EDGE('',*,*,#7663,.F.);
#10080=ORIENTED_EDGE('',*,*,#7662,.T.);
#10081=ORIENTED_EDGE('',*,*,#7664,.F.);
#10082=ORIENTED_EDGE('',*,*,#7665,.F.);
#10083=ORIENTED_EDGE('',*,*,#7666,.F.);
#10084=ORIENTED_EDGE('',*,*,#7665,.T.);
#10085=ORIENTED_EDGE('',*,*,#7667,.F.);
#10086=ORIENTED_EDGE('',*,*,#7668,.F.);
#10087=ORIENTED_EDGE('',*,*,#7669,.F.);
#10088=ORIENTED_EDGE('',*,*,#7668,.T.);
#10089=ORIENTED_EDGE('',*,*,#7670,.F.);
#10090=ORIENTED_EDGE('',*,*,#7671,.F.);
#10091=ORIENTED_EDGE('',*,*,#7672,.F.);
#10092=ORIENTED_EDGE('',*,*,#7671,.T.);
#10093=ORIENTED_EDGE('',*,*,#7673,.F.);
#10094=ORIENTED_EDGE('',*,*,#7674,.F.);
#10095=ORIENTED_EDGE('',*,*,#7675,.F.);
#10096=ORIENTED_EDGE('',*,*,#7674,.T.);
#10097=ORIENTED_EDGE('',*,*,#7676,.F.);
#10098=ORIENTED_EDGE('',*,*,#7677,.F.);
#10099=ORIENTED_EDGE('',*,*,#7678,.F.);
#10100=ORIENTED_EDGE('',*,*,#7677,.T.);
#10101=ORIENTED_EDGE('',*,*,#7679,.F.);
#10102=ORIENTED_EDGE('',*,*,#7680,.F.);
#10103=ORIENTED_EDGE('',*,*,#7681,.F.);
#10104=ORIENTED_EDGE('',*,*,#7680,.T.);
#10105=ORIENTED_EDGE('',*,*,#7682,.F.);
#10106=ORIENTED_EDGE('',*,*,#7683,.F.);
#10107=ORIENTED_EDGE('',*,*,#7684,.F.);
#10108=ORIENTED_EDGE('',*,*,#7683,.T.);
#10109=ORIENTED_EDGE('',*,*,#7685,.F.);
#10110=ORIENTED_EDGE('',*,*,#7686,.F.);
#10111=ORIENTED_EDGE('',*,*,#7687,.F.);
#10112=ORIENTED_EDGE('',*,*,#7686,.T.);
#10113=ORIENTED_EDGE('',*,*,#7688,.F.);
#10114=ORIENTED_EDGE('',*,*,#7689,.F.);
#10115=ORIENTED_EDGE('',*,*,#7690,.F.);
#10116=ORIENTED_EDGE('',*,*,#7689,.T.);
#10117=ORIENTED_EDGE('',*,*,#7691,.F.);
#10118=ORIENTED_EDGE('',*,*,#7692,.F.);
#10119=ORIENTED_EDGE('',*,*,#7693,.F.);
#10120=ORIENTED_EDGE('',*,*,#7692,.T.);
#10121=ORIENTED_EDGE('',*,*,#7694,.F.);
#10122=ORIENTED_EDGE('',*,*,#7695,.F.);
#10123=ORIENTED_EDGE('',*,*,#7696,.F.);
#10124=ORIENTED_EDGE('',*,*,#7695,.T.);
#10125=ORIENTED_EDGE('',*,*,#7697,.F.);
#10126=ORIENTED_EDGE('',*,*,#7698,.F.);
#10127=ORIENTED_EDGE('',*,*,#7699,.F.);
#10128=ORIENTED_EDGE('',*,*,#7698,.T.);
#10129=ORIENTED_EDGE('',*,*,#7700,.F.);
#10130=ORIENTED_EDGE('',*,*,#7701,.F.);
#10131=ORIENTED_EDGE('',*,*,#7702,.F.);
#10132=ORIENTED_EDGE('',*,*,#7701,.T.);
#10133=ORIENTED_EDGE('',*,*,#7703,.F.);
#10134=ORIENTED_EDGE('',*,*,#7704,.F.);
#10135=ORIENTED_EDGE('',*,*,#7705,.F.);
#10136=ORIENTED_EDGE('',*,*,#7704,.T.);
#10137=ORIENTED_EDGE('',*,*,#7706,.F.);
#10138=ORIENTED_EDGE('',*,*,#7707,.F.);
#10139=ORIENTED_EDGE('',*,*,#7708,.F.);
#10140=ORIENTED_EDGE('',*,*,#7707,.T.);
#10141=ORIENTED_EDGE('',*,*,#7709,.F.);
#10142=ORIENTED_EDGE('',*,*,#7710,.F.);
#10143=ORIENTED_EDGE('',*,*,#7711,.F.);
#10144=ORIENTED_EDGE('',*,*,#7710,.T.);
#10145=ORIENTED_EDGE('',*,*,#7712,.F.);
#10146=ORIENTED_EDGE('',*,*,#7713,.F.);
#10147=ORIENTED_EDGE('',*,*,#7714,.F.);
#10148=ORIENTED_EDGE('',*,*,#7713,.T.);
#10149=ORIENTED_EDGE('',*,*,#7715,.F.);
#10150=ORIENTED_EDGE('',*,*,#7716,.F.);
#10151=ORIENTED_EDGE('',*,*,#7717,.F.);
#10152=ORIENTED_EDGE('',*,*,#7716,.T.);
#10153=ORIENTED_EDGE('',*,*,#7718,.F.);
#10154=ORIENTED_EDGE('',*,*,#7719,.F.);
#10155=ORIENTED_EDGE('',*,*,#7720,.F.);
#10156=ORIENTED_EDGE('',*,*,#7719,.T.);
#10157=ORIENTED_EDGE('',*,*,#7721,.F.);
#10158=ORIENTED_EDGE('',*,*,#7722,.F.);
#10159=ORIENTED_EDGE('',*,*,#7723,.F.);
#10160=ORIENTED_EDGE('',*,*,#7722,.T.);
#10161=ORIENTED_EDGE('',*,*,#7724,.F.);
#10162=ORIENTED_EDGE('',*,*,#7725,.F.);
#10163=ORIENTED_EDGE('',*,*,#7726,.F.);
#10164=ORIENTED_EDGE('',*,*,#7725,.T.);
#10165=ORIENTED_EDGE('',*,*,#7727,.F.);
#10166=ORIENTED_EDGE('',*,*,#7728,.F.);
#10167=ORIENTED_EDGE('',*,*,#7729,.F.);
#10168=ORIENTED_EDGE('',*,*,#7728,.T.);
#10169=ORIENTED_EDGE('',*,*,#7730,.F.);
#10170=ORIENTED_EDGE('',*,*,#7731,.F.);
#10171=ORIENTED_EDGE('',*,*,#7732,.F.);
#10172=ORIENTED_EDGE('',*,*,#7731,.T.);
#10173=ORIENTED_EDGE('',*,*,#7733,.F.);
#10174=ORIENTED_EDGE('',*,*,#7734,.F.);
#10175=ORIENTED_EDGE('',*,*,#7735,.F.);
#10176=ORIENTED_EDGE('',*,*,#7734,.T.);
#10177=ORIENTED_EDGE('',*,*,#7736,.F.);
#10178=ORIENTED_EDGE('',*,*,#7737,.F.);
#10179=ORIENTED_EDGE('',*,*,#7738,.F.);
#10180=ORIENTED_EDGE('',*,*,#7737,.T.);
#10181=ORIENTED_EDGE('',*,*,#7739,.F.);
#10182=ORIENTED_EDGE('',*,*,#7740,.F.);
#10183=ORIENTED_EDGE('',*,*,#7741,.F.);
#10184=ORIENTED_EDGE('',*,*,#7740,.T.);
#10185=ORIENTED_EDGE('',*,*,#7742,.F.);
#10186=ORIENTED_EDGE('',*,*,#7743,.F.);
#10187=ORIENTED_EDGE('',*,*,#7744,.F.);
#10188=ORIENTED_EDGE('',*,*,#7743,.T.);
#10189=ORIENTED_EDGE('',*,*,#7745,.F.);
#10190=ORIENTED_EDGE('',*,*,#7746,.F.);
#10191=ORIENTED_EDGE('',*,*,#7747,.F.);
#10192=ORIENTED_EDGE('',*,*,#7746,.T.);
#10193=ORIENTED_EDGE('',*,*,#7748,.F.);
#10194=ORIENTED_EDGE('',*,*,#7749,.F.);
#10195=ORIENTED_EDGE('',*,*,#7750,.F.);
#10196=ORIENTED_EDGE('',*,*,#7749,.T.);
#10197=ORIENTED_EDGE('',*,*,#7751,.F.);
#10198=ORIENTED_EDGE('',*,*,#7752,.F.);
#10199=ORIENTED_EDGE('',*,*,#7753,.F.);
#10200=ORIENTED_EDGE('',*,*,#7752,.T.);
#10201=ORIENTED_EDGE('',*,*,#7754,.F.);
#10202=ORIENTED_EDGE('',*,*,#7755,.F.);
#10203=ORIENTED_EDGE('',*,*,#7756,.F.);
#10204=ORIENTED_EDGE('',*,*,#7755,.T.);
#10205=ORIENTED_EDGE('',*,*,#7757,.F.);
#10206=ORIENTED_EDGE('',*,*,#7758,.F.);
#10207=ORIENTED_EDGE('',*,*,#7759,.F.);
#10208=ORIENTED_EDGE('',*,*,#7758,.T.);
#10209=ORIENTED_EDGE('',*,*,#7760,.F.);
#10210=ORIENTED_EDGE('',*,*,#7761,.F.);
#10211=ORIENTED_EDGE('',*,*,#7762,.F.);
#10212=ORIENTED_EDGE('',*,*,#7761,.T.);
#10213=ORIENTED_EDGE('',*,*,#7763,.F.);
#10214=ORIENTED_EDGE('',*,*,#7764,.F.);
#10215=ORIENTED_EDGE('',*,*,#7765,.F.);
#10216=ORIENTED_EDGE('',*,*,#7764,.T.);
#10217=ORIENTED_EDGE('',*,*,#7766,.F.);
#10218=ORIENTED_EDGE('',*,*,#7767,.F.);
#10219=ORIENTED_EDGE('',*,*,#7768,.F.);
#10220=ORIENTED_EDGE('',*,*,#7767,.T.);
#10221=ORIENTED_EDGE('',*,*,#7769,.F.);
#10222=ORIENTED_EDGE('',*,*,#7770,.F.);
#10223=ORIENTED_EDGE('',*,*,#7771,.F.);
#10224=ORIENTED_EDGE('',*,*,#7770,.T.);
#10225=ORIENTED_EDGE('',*,*,#7772,.F.);
#10226=ORIENTED_EDGE('',*,*,#7773,.F.);
#10227=ORIENTED_EDGE('',*,*,#7774,.F.);
#10228=ORIENTED_EDGE('',*,*,#7773,.T.);
#10229=ORIENTED_EDGE('',*,*,#7775,.F.);
#10230=ORIENTED_EDGE('',*,*,#7776,.F.);
#10231=ORIENTED_EDGE('',*,*,#7777,.F.);
#10232=ORIENTED_EDGE('',*,*,#7776,.T.);
#10233=ORIENTED_EDGE('',*,*,#7778,.F.);
#10234=ORIENTED_EDGE('',*,*,#7779,.F.);
#10235=ORIENTED_EDGE('',*,*,#7780,.F.);
#10236=ORIENTED_EDGE('',*,*,#7779,.T.);
#10237=ORIENTED_EDGE('',*,*,#7781,.F.);
#10238=ORIENTED_EDGE('',*,*,#7782,.F.);
#10239=ORIENTED_EDGE('',*,*,#7783,.F.);
#10240=ORIENTED_EDGE('',*,*,#7782,.T.);
#10241=ORIENTED_EDGE('',*,*,#7784,.F.);
#10242=ORIENTED_EDGE('',*,*,#7785,.F.);
#10243=ORIENTED_EDGE('',*,*,#7786,.F.);
#10244=ORIENTED_EDGE('',*,*,#7785,.T.);
#10245=ORIENTED_EDGE('',*,*,#7787,.F.);
#10246=ORIENTED_EDGE('',*,*,#7788,.F.);
#10247=ORIENTED_EDGE('',*,*,#7789,.F.);
#10248=ORIENTED_EDGE('',*,*,#7788,.T.);
#10249=ORIENTED_EDGE('',*,*,#7790,.F.);
#10250=ORIENTED_EDGE('',*,*,#7791,.F.);
#10251=ORIENTED_EDGE('',*,*,#7792,.F.);
#10252=ORIENTED_EDGE('',*,*,#7791,.T.);
#10253=ORIENTED_EDGE('',*,*,#7793,.F.);
#10254=ORIENTED_EDGE('',*,*,#7794,.F.);
#10255=ORIENTED_EDGE('',*,*,#7795,.F.);
#10256=ORIENTED_EDGE('',*,*,#7794,.T.);
#10257=ORIENTED_EDGE('',*,*,#7796,.F.);
#10258=ORIENTED_EDGE('',*,*,#7797,.F.);
#10259=ORIENTED_EDGE('',*,*,#7798,.F.);
#10260=ORIENTED_EDGE('',*,*,#7797,.T.);
#10261=ORIENTED_EDGE('',*,*,#7799,.F.);
#10262=ORIENTED_EDGE('',*,*,#7800,.F.);
#10263=ORIENTED_EDGE('',*,*,#7801,.F.);
#10264=ORIENTED_EDGE('',*,*,#7800,.T.);
#10265=ORIENTED_EDGE('',*,*,#7802,.F.);
#10266=ORIENTED_EDGE('',*,*,#7803,.F.);
#10267=ORIENTED_EDGE('',*,*,#7804,.F.);
#10268=ORIENTED_EDGE('',*,*,#7803,.T.);
#10269=ORIENTED_EDGE('',*,*,#7805,.F.);
#10270=ORIENTED_EDGE('',*,*,#7316,.F.);
#10271=ORIENTED_EDGE('',*,*,#7805,.T.);
#10272=ORIENTED_EDGE('',*,*,#7802,.T.);
#10273=ORIENTED_EDGE('',*,*,#7799,.T.);
#10274=ORIENTED_EDGE('',*,*,#7796,.T.);
#10275=ORIENTED_EDGE('',*,*,#7793,.T.);
#10276=ORIENTED_EDGE('',*,*,#7790,.T.);
#10277=ORIENTED_EDGE('',*,*,#7787,.T.);
#10278=ORIENTED_EDGE('',*,*,#7784,.T.);
#10279=ORIENTED_EDGE('',*,*,#7781,.T.);
#10280=ORIENTED_EDGE('',*,*,#7778,.T.);
#10281=ORIENTED_EDGE('',*,*,#7775,.T.);
#10282=ORIENTED_EDGE('',*,*,#7772,.T.);
#10283=ORIENTED_EDGE('',*,*,#7769,.T.);
#10284=ORIENTED_EDGE('',*,*,#7766,.T.);
#10285=ORIENTED_EDGE('',*,*,#7763,.T.);
#10286=ORIENTED_EDGE('',*,*,#7760,.T.);
#10287=ORIENTED_EDGE('',*,*,#7757,.T.);
#10288=ORIENTED_EDGE('',*,*,#7754,.T.);
#10289=ORIENTED_EDGE('',*,*,#7751,.T.);
#10290=ORIENTED_EDGE('',*,*,#7748,.T.);
#10291=ORIENTED_EDGE('',*,*,#7745,.T.);
#10292=ORIENTED_EDGE('',*,*,#7742,.T.);
#10293=ORIENTED_EDGE('',*,*,#7739,.T.);
#10294=ORIENTED_EDGE('',*,*,#7736,.T.);
#10295=ORIENTED_EDGE('',*,*,#7733,.T.);
#10296=ORIENTED_EDGE('',*,*,#7730,.T.);
#10297=ORIENTED_EDGE('',*,*,#7727,.T.);
#10298=ORIENTED_EDGE('',*,*,#7724,.T.);
#10299=ORIENTED_EDGE('',*,*,#7721,.T.);
#10300=ORIENTED_EDGE('',*,*,#7718,.T.);
#10301=ORIENTED_EDGE('',*,*,#7715,.T.);
#10302=ORIENTED_EDGE('',*,*,#7712,.T.);
#10303=ORIENTED_EDGE('',*,*,#7709,.T.);
#10304=ORIENTED_EDGE('',*,*,#7706,.T.);
#10305=ORIENTED_EDGE('',*,*,#7703,.T.);
#10306=ORIENTED_EDGE('',*,*,#7700,.T.);
#10307=ORIENTED_EDGE('',*,*,#7697,.T.);
#10308=ORIENTED_EDGE('',*,*,#7694,.T.);
#10309=ORIENTED_EDGE('',*,*,#7691,.T.);
#10310=ORIENTED_EDGE('',*,*,#7688,.T.);
#10311=ORIENTED_EDGE('',*,*,#7685,.T.);
#10312=ORIENTED_EDGE('',*,*,#7682,.T.);
#10313=ORIENTED_EDGE('',*,*,#7679,.T.);
#10314=ORIENTED_EDGE('',*,*,#7676,.T.);
#10315=ORIENTED_EDGE('',*,*,#7673,.T.);
#10316=ORIENTED_EDGE('',*,*,#7670,.T.);
#10317=ORIENTED_EDGE('',*,*,#7667,.T.);
#10318=ORIENTED_EDGE('',*,*,#7664,.T.);
#10319=ORIENTED_EDGE('',*,*,#7661,.T.);
#10320=ORIENTED_EDGE('',*,*,#7658,.T.);
#10321=ORIENTED_EDGE('',*,*,#7655,.T.);
#10322=ORIENTED_EDGE('',*,*,#7652,.T.);
#10323=ORIENTED_EDGE('',*,*,#7649,.T.);
#10324=ORIENTED_EDGE('',*,*,#7646,.T.);
#10325=ORIENTED_EDGE('',*,*,#7643,.T.);
#10326=ORIENTED_EDGE('',*,*,#7640,.T.);
#10327=ORIENTED_EDGE('',*,*,#7637,.T.);
#10328=ORIENTED_EDGE('',*,*,#7634,.T.);
#10329=ORIENTED_EDGE('',*,*,#7631,.T.);
#10330=ORIENTED_EDGE('',*,*,#7628,.T.);
#10331=ORIENTED_EDGE('',*,*,#7625,.T.);
#10332=ORIENTED_EDGE('',*,*,#7622,.T.);
#10333=ORIENTED_EDGE('',*,*,#7619,.T.);
#10334=ORIENTED_EDGE('',*,*,#7616,.T.);
#10335=ORIENTED_EDGE('',*,*,#7613,.T.);
#10336=ORIENTED_EDGE('',*,*,#7610,.T.);
#10337=ORIENTED_EDGE('',*,*,#7607,.T.);
#10338=ORIENTED_EDGE('',*,*,#7604,.T.);
#10339=ORIENTED_EDGE('',*,*,#7601,.T.);
#10340=ORIENTED_EDGE('',*,*,#7598,.T.);
#10341=ORIENTED_EDGE('',*,*,#7595,.T.);
#10342=ORIENTED_EDGE('',*,*,#7592,.T.);
#10343=ORIENTED_EDGE('',*,*,#7589,.T.);
#10344=ORIENTED_EDGE('',*,*,#7586,.T.);
#10345=ORIENTED_EDGE('',*,*,#7583,.T.);
#10346=ORIENTED_EDGE('',*,*,#7580,.T.);
#10347=ORIENTED_EDGE('',*,*,#7577,.T.);
#10348=ORIENTED_EDGE('',*,*,#7574,.T.);
#10349=ORIENTED_EDGE('',*,*,#7571,.T.);
#10350=ORIENTED_EDGE('',*,*,#7568,.T.);
#10351=ORIENTED_EDGE('',*,*,#7565,.T.);
#10352=ORIENTED_EDGE('',*,*,#7562,.T.);
#10353=ORIENTED_EDGE('',*,*,#7559,.T.);
#10354=ORIENTED_EDGE('',*,*,#7556,.T.);
#10355=ORIENTED_EDGE('',*,*,#7553,.T.);
#10356=ORIENTED_EDGE('',*,*,#7550,.T.);
#10357=ORIENTED_EDGE('',*,*,#7547,.T.);
#10358=ORIENTED_EDGE('',*,*,#7544,.T.);
#10359=ORIENTED_EDGE('',*,*,#7541,.T.);
#10360=ORIENTED_EDGE('',*,*,#7538,.T.);
#10361=ORIENTED_EDGE('',*,*,#7535,.T.);
#10362=ORIENTED_EDGE('',*,*,#7532,.T.);
#10363=ORIENTED_EDGE('',*,*,#7529,.T.);
#10364=ORIENTED_EDGE('',*,*,#7526,.T.);
#10365=ORIENTED_EDGE('',*,*,#7523,.T.);
#10366=ORIENTED_EDGE('',*,*,#7520,.T.);
#10367=ORIENTED_EDGE('',*,*,#7517,.T.);
#10368=ORIENTED_EDGE('',*,*,#7514,.T.);
#10369=ORIENTED_EDGE('',*,*,#7511,.T.);
#10370=ORIENTED_EDGE('',*,*,#7508,.T.);
#10371=ORIENTED_EDGE('',*,*,#7505,.T.);
#10372=ORIENTED_EDGE('',*,*,#7502,.T.);
#10373=ORIENTED_EDGE('',*,*,#7499,.T.);
#10374=ORIENTED_EDGE('',*,*,#7496,.T.);
#10375=ORIENTED_EDGE('',*,*,#7493,.T.);
#10376=ORIENTED_EDGE('',*,*,#7490,.T.);
#10377=ORIENTED_EDGE('',*,*,#7487,.T.);
#10378=ORIENTED_EDGE('',*,*,#7484,.T.);
#10379=ORIENTED_EDGE('',*,*,#7481,.T.);
#10380=ORIENTED_EDGE('',*,*,#7478,.T.);
#10381=ORIENTED_EDGE('',*,*,#7475,.T.);
#10382=ORIENTED_EDGE('',*,*,#7472,.T.);
#10383=ORIENTED_EDGE('',*,*,#7469,.T.);
#10384=ORIENTED_EDGE('',*,*,#7466,.T.);
#10385=ORIENTED_EDGE('',*,*,#7463,.T.);
#10386=ORIENTED_EDGE('',*,*,#7460,.T.);
#10387=ORIENTED_EDGE('',*,*,#7457,.T.);
#10388=ORIENTED_EDGE('',*,*,#7454,.T.);
#10389=ORIENTED_EDGE('',*,*,#7451,.T.);
#10390=ORIENTED_EDGE('',*,*,#7448,.T.);
#10391=ORIENTED_EDGE('',*,*,#7445,.T.);
#10392=ORIENTED_EDGE('',*,*,#7442,.T.);
#10393=ORIENTED_EDGE('',*,*,#7439,.T.);
#10394=ORIENTED_EDGE('',*,*,#7436,.T.);
#10395=ORIENTED_EDGE('',*,*,#7433,.T.);
#10396=ORIENTED_EDGE('',*,*,#7430,.T.);
#10397=ORIENTED_EDGE('',*,*,#7427,.T.);
#10398=ORIENTED_EDGE('',*,*,#7424,.T.);
#10399=ORIENTED_EDGE('',*,*,#7421,.T.);
#10400=ORIENTED_EDGE('',*,*,#7418,.T.);
#10401=ORIENTED_EDGE('',*,*,#7415,.T.);
#10402=ORIENTED_EDGE('',*,*,#7412,.T.);
#10403=ORIENTED_EDGE('',*,*,#7409,.T.);
#10404=ORIENTED_EDGE('',*,*,#7406,.T.);
#10405=ORIENTED_EDGE('',*,*,#7403,.T.);
#10406=ORIENTED_EDGE('',*,*,#7400,.T.);
#10407=ORIENTED_EDGE('',*,*,#7397,.T.);
#10408=ORIENTED_EDGE('',*,*,#7394,.T.);
#10409=ORIENTED_EDGE('',*,*,#7391,.T.);
#10410=ORIENTED_EDGE('',*,*,#7388,.T.);
#10411=ORIENTED_EDGE('',*,*,#7385,.T.);
#10412=ORIENTED_EDGE('',*,*,#7382,.T.);
#10413=ORIENTED_EDGE('',*,*,#7379,.T.);
#10414=ORIENTED_EDGE('',*,*,#7376,.T.);
#10415=ORIENTED_EDGE('',*,*,#7373,.T.);
#10416=ORIENTED_EDGE('',*,*,#7370,.T.);
#10417=ORIENTED_EDGE('',*,*,#7367,.T.);
#10418=ORIENTED_EDGE('',*,*,#7364,.T.);
#10419=ORIENTED_EDGE('',*,*,#7361,.T.);
#10420=ORIENTED_EDGE('',*,*,#7358,.T.);
#10421=ORIENTED_EDGE('',*,*,#7355,.T.);
#10422=ORIENTED_EDGE('',*,*,#7352,.T.);
#10423=ORIENTED_EDGE('',*,*,#7349,.T.);
#10424=ORIENTED_EDGE('',*,*,#7346,.T.);
#10425=ORIENTED_EDGE('',*,*,#7343,.T.);
#10426=ORIENTED_EDGE('',*,*,#7340,.T.);
#10427=ORIENTED_EDGE('',*,*,#7337,.T.);
#10428=ORIENTED_EDGE('',*,*,#7334,.T.);
#10429=ORIENTED_EDGE('',*,*,#7331,.T.);
#10430=ORIENTED_EDGE('',*,*,#7328,.T.);
#10431=ORIENTED_EDGE('',*,*,#7325,.T.);
#10432=ORIENTED_EDGE('',*,*,#7320,.T.);
#10433=ORIENTED_EDGE('',*,*,#7312,.T.);
#10434=ORIENTED_EDGE('',*,*,#7317,.T.);
#10435=ORIENTED_EDGE('',*,*,#7804,.T.);
#10436=ORIENTED_EDGE('',*,*,#7315,.T.);
#10437=ORIENTED_EDGE('',*,*,#7308,.T.);
#10438=ORIENTED_EDGE('',*,*,#7322,.T.);
#10439=ORIENTED_EDGE('',*,*,#7324,.T.);
#10440=ORIENTED_EDGE('',*,*,#7327,.T.);
#10441=ORIENTED_EDGE('',*,*,#7330,.T.);
#10442=ORIENTED_EDGE('',*,*,#7333,.T.);
#10443=ORIENTED_EDGE('',*,*,#7336,.T.);
#10444=ORIENTED_EDGE('',*,*,#7339,.T.);
#10445=ORIENTED_EDGE('',*,*,#7342,.T.);
#10446=ORIENTED_EDGE('',*,*,#7345,.T.);
#10447=ORIENTED_EDGE('',*,*,#7348,.T.);
#10448=ORIENTED_EDGE('',*,*,#7351,.T.);
#10449=ORIENTED_EDGE('',*,*,#7354,.T.);
#10450=ORIENTED_EDGE('',*,*,#7357,.T.);
#10451=ORIENTED_EDGE('',*,*,#7360,.T.);
#10452=ORIENTED_EDGE('',*,*,#7363,.T.);
#10453=ORIENTED_EDGE('',*,*,#7366,.T.);
#10454=ORIENTED_EDGE('',*,*,#7369,.T.);
#10455=ORIENTED_EDGE('',*,*,#7372,.T.);
#10456=ORIENTED_EDGE('',*,*,#7375,.T.);
#10457=ORIENTED_EDGE('',*,*,#7378,.T.);
#10458=ORIENTED_EDGE('',*,*,#7381,.T.);
#10459=ORIENTED_EDGE('',*,*,#7384,.T.);
#10460=ORIENTED_EDGE('',*,*,#7387,.T.);
#10461=ORIENTED_EDGE('',*,*,#7390,.T.);
#10462=ORIENTED_EDGE('',*,*,#7393,.T.);
#10463=ORIENTED_EDGE('',*,*,#7396,.T.);
#10464=ORIENTED_EDGE('',*,*,#7399,.T.);
#10465=ORIENTED_EDGE('',*,*,#7402,.T.);
#10466=ORIENTED_EDGE('',*,*,#7405,.T.);
#10467=ORIENTED_EDGE('',*,*,#7408,.T.);
#10468=ORIENTED_EDGE('',*,*,#7411,.T.);
#10469=ORIENTED_EDGE('',*,*,#7414,.T.);
#10470=ORIENTED_EDGE('',*,*,#7417,.T.);
#10471=ORIENTED_EDGE('',*,*,#7420,.T.);
#10472=ORIENTED_EDGE('',*,*,#7423,.T.);
#10473=ORIENTED_EDGE('',*,*,#7426,.T.);
#10474=ORIENTED_EDGE('',*,*,#7429,.T.);
#10475=ORIENTED_EDGE('',*,*,#7432,.T.);
#10476=ORIENTED_EDGE('',*,*,#7435,.T.);
#10477=ORIENTED_EDGE('',*,*,#7438,.T.);
#10478=ORIENTED_EDGE('',*,*,#7441,.T.);
#10479=ORIENTED_EDGE('',*,*,#7444,.T.);
#10480=ORIENTED_EDGE('',*,*,#7447,.T.);
#10481=ORIENTED_EDGE('',*,*,#7450,.T.);
#10482=ORIENTED_EDGE('',*,*,#7453,.T.);
#10483=ORIENTED_EDGE('',*,*,#7456,.T.);
#10484=ORIENTED_EDGE('',*,*,#7459,.T.);
#10485=ORIENTED_EDGE('',*,*,#7462,.T.);
#10486=ORIENTED_EDGE('',*,*,#7465,.T.);
#10487=ORIENTED_EDGE('',*,*,#7468,.T.);
#10488=ORIENTED_EDGE('',*,*,#7471,.T.);
#10489=ORIENTED_EDGE('',*,*,#7474,.T.);
#10490=ORIENTED_EDGE('',*,*,#7477,.T.);
#10491=ORIENTED_EDGE('',*,*,#7480,.T.);
#10492=ORIENTED_EDGE('',*,*,#7483,.T.);
#10493=ORIENTED_EDGE('',*,*,#7486,.T.);
#10494=ORIENTED_EDGE('',*,*,#7489,.T.);
#10495=ORIENTED_EDGE('',*,*,#7492,.T.);
#10496=ORIENTED_EDGE('',*,*,#7495,.T.);
#10497=ORIENTED_EDGE('',*,*,#7498,.T.);
#10498=ORIENTED_EDGE('',*,*,#7501,.T.);
#10499=ORIENTED_EDGE('',*,*,#7504,.T.);
#10500=ORIENTED_EDGE('',*,*,#7507,.T.);
#10501=ORIENTED_EDGE('',*,*,#7510,.T.);
#10502=ORIENTED_EDGE('',*,*,#7513,.T.);
#10503=ORIENTED_EDGE('',*,*,#7516,.T.);
#10504=ORIENTED_EDGE('',*,*,#7519,.T.);
#10505=ORIENTED_EDGE('',*,*,#7522,.T.);
#10506=ORIENTED_EDGE('',*,*,#7525,.T.);
#10507=ORIENTED_EDGE('',*,*,#7528,.T.);
#10508=ORIENTED_EDGE('',*,*,#7531,.T.);
#10509=ORIENTED_EDGE('',*,*,#7534,.T.);
#10510=ORIENTED_EDGE('',*,*,#7537,.T.);
#10511=ORIENTED_EDGE('',*,*,#7540,.T.);
#10512=ORIENTED_EDGE('',*,*,#7543,.T.);
#10513=ORIENTED_EDGE('',*,*,#7546,.T.);
#10514=ORIENTED_EDGE('',*,*,#7549,.T.);
#10515=ORIENTED_EDGE('',*,*,#7552,.T.);
#10516=ORIENTED_EDGE('',*,*,#7555,.T.);
#10517=ORIENTED_EDGE('',*,*,#7558,.T.);
#10518=ORIENTED_EDGE('',*,*,#7561,.T.);
#10519=ORIENTED_EDGE('',*,*,#7564,.T.);
#10520=ORIENTED_EDGE('',*,*,#7567,.T.);
#10521=ORIENTED_EDGE('',*,*,#7570,.T.);
#10522=ORIENTED_EDGE('',*,*,#7573,.T.);
#10523=ORIENTED_EDGE('',*,*,#7576,.T.);
#10524=ORIENTED_EDGE('',*,*,#7579,.T.);
#10525=ORIENTED_EDGE('',*,*,#7582,.T.);
#10526=ORIENTED_EDGE('',*,*,#7585,.T.);
#10527=ORIENTED_EDGE('',*,*,#7588,.T.);
#10528=ORIENTED_EDGE('',*,*,#7591,.T.);
#10529=ORIENTED_EDGE('',*,*,#7594,.T.);
#10530=ORIENTED_EDGE('',*,*,#7597,.T.);
#10531=ORIENTED_EDGE('',*,*,#7600,.T.);
#10532=ORIENTED_EDGE('',*,*,#7603,.T.);
#10533=ORIENTED_EDGE('',*,*,#7606,.T.);
#10534=ORIENTED_EDGE('',*,*,#7609,.T.);
#10535=ORIENTED_EDGE('',*,*,#7612,.T.);
#10536=ORIENTED_EDGE('',*,*,#7615,.T.);
#10537=ORIENTED_EDGE('',*,*,#7618,.T.);
#10538=ORIENTED_EDGE('',*,*,#7621,.T.);
#10539=ORIENTED_EDGE('',*,*,#7624,.T.);
#10540=ORIENTED_EDGE('',*,*,#7627,.T.);
#10541=ORIENTED_EDGE('',*,*,#7630,.T.);
#10542=ORIENTED_EDGE('',*,*,#7633,.T.);
#10543=ORIENTED_EDGE('',*,*,#7636,.T.);
#10544=ORIENTED_EDGE('',*,*,#7639,.T.);
#10545=ORIENTED_EDGE('',*,*,#7642,.T.);
#10546=ORIENTED_EDGE('',*,*,#7645,.T.);
#10547=ORIENTED_EDGE('',*,*,#7648,.T.);
#10548=ORIENTED_EDGE('',*,*,#7651,.T.);
#10549=ORIENTED_EDGE('',*,*,#7654,.T.);
#10550=ORIENTED_EDGE('',*,*,#7657,.T.);
#10551=ORIENTED_EDGE('',*,*,#7660,.T.);
#10552=ORIENTED_EDGE('',*,*,#7663,.T.);
#10553=ORIENTED_EDGE('',*,*,#7666,.T.);
#10554=ORIENTED_EDGE('',*,*,#7669,.T.);
#10555=ORIENTED_EDGE('',*,*,#7672,.T.);
#10556=ORIENTED_EDGE('',*,*,#7675,.T.);
#10557=ORIENTED_EDGE('',*,*,#7678,.T.);
#10558=ORIENTED_EDGE('',*,*,#7681,.T.);
#10559=ORIENTED_EDGE('',*,*,#7684,.T.);
#10560=ORIENTED_EDGE('',*,*,#7687,.T.);
#10561=ORIENTED_EDGE('',*,*,#7690,.T.);
#10562=ORIENTED_EDGE('',*,*,#7693,.T.);
#10563=ORIENTED_EDGE('',*,*,#7696,.T.);
#10564=ORIENTED_EDGE('',*,*,#7699,.T.);
#10565=ORIENTED_EDGE('',*,*,#7702,.T.);
#10566=ORIENTED_EDGE('',*,*,#7705,.T.);
#10567=ORIENTED_EDGE('',*,*,#7708,.T.);
#10568=ORIENTED_EDGE('',*,*,#7711,.T.);
#10569=ORIENTED_EDGE('',*,*,#7714,.T.);
#10570=ORIENTED_EDGE('',*,*,#7717,.T.);
#10571=ORIENTED_EDGE('',*,*,#7720,.T.);
#10572=ORIENTED_EDGE('',*,*,#7723,.T.);
#10573=ORIENTED_EDGE('',*,*,#7726,.T.);
#10574=ORIENTED_EDGE('',*,*,#7729,.T.);
#10575=ORIENTED_EDGE('',*,*,#7732,.T.);
#10576=ORIENTED_EDGE('',*,*,#7735,.T.);
#10577=ORIENTED_EDGE('',*,*,#7738,.T.);
#10578=ORIENTED_EDGE('',*,*,#7741,.T.);
#10579=ORIENTED_EDGE('',*,*,#7744,.T.);
#10580=ORIENTED_EDGE('',*,*,#7747,.T.);
#10581=ORIENTED_EDGE('',*,*,#7750,.T.);
#10582=ORIENTED_EDGE('',*,*,#7753,.T.);
#10583=ORIENTED_EDGE('',*,*,#7756,.T.);
#10584=ORIENTED_EDGE('',*,*,#7759,.T.);
#10585=ORIENTED_EDGE('',*,*,#7762,.T.);
#10586=ORIENTED_EDGE('',*,*,#7765,.T.);
#10587=ORIENTED_EDGE('',*,*,#7768,.T.);
#10588=ORIENTED_EDGE('',*,*,#7771,.T.);
#10589=ORIENTED_EDGE('',*,*,#7774,.T.);
#10590=ORIENTED_EDGE('',*,*,#7777,.T.);
#10591=ORIENTED_EDGE('',*,*,#7780,.T.);
#10592=ORIENTED_EDGE('',*,*,#7783,.T.);
#10593=ORIENTED_EDGE('',*,*,#7786,.T.);
#10594=ORIENTED_EDGE('',*,*,#7789,.T.);
#10595=ORIENTED_EDGE('',*,*,#7792,.T.);
#10596=ORIENTED_EDGE('',*,*,#7795,.T.);
#10597=ORIENTED_EDGE('',*,*,#7798,.T.);
#10598=ORIENTED_EDGE('',*,*,#7801,.T.);
#10599=ORIENTED_EDGE('',*,*,#7806,.F.);
#10600=ORIENTED_EDGE('',*,*,#7807,.T.);
#10601=ORIENTED_EDGE('',*,*,#7323,.T.);
#10602=ORIENTED_EDGE('',*,*,#7306,.T.);
#10603=ORIENTED_EDGE('',*,*,#7314,.T.);
#10604=ORIENTED_EDGE('',*,*,#7808,.T.);
#10605=ORIENTED_EDGE('',*,*,#7809,.T.);
#10606=ORIENTED_EDGE('',*,*,#7808,.F.);
#10607=ORIENTED_EDGE('',*,*,#7318,.T.);
#10608=ORIENTED_EDGE('',*,*,#7310,.T.);
#10609=ORIENTED_EDGE('',*,*,#7319,.T.);
#10610=ORIENTED_EDGE('',*,*,#7807,.F.);
#10611=ORIENTED_EDGE('',*,*,#7806,.T.);
#10612=ORIENTED_EDGE('',*,*,#7809,.F.);
#10613=ORIENTED_EDGE('',*,*,#7303,.T.);
#10614=ORIENTED_EDGE('',*,*,#7810,.F.);
#10615=ORIENTED_EDGE('',*,*,#7811,.T.);
#10616=ORIENTED_EDGE('',*,*,#7812,.F.);
#10617=ORIENTED_EDGE('',*,*,#7811,.F.);
#10618=ORIENTED_EDGE('',*,*,#7810,.T.);
#10619=ORIENTED_EDGE('',*,*,#7813,.F.);
#10620=ORIENTED_EDGE('',*,*,#7814,.T.);
#10621=ORIENTED_EDGE('',*,*,#7815,.T.);
#10622=ORIENTED_EDGE('',*,*,#7814,.F.);
#10623=ORIENTED_EDGE('',*,*,#7813,.T.);
#10624=ORIENTED_EDGE('',*,*,#7812,.T.);
#10625=ORIENTED_EDGE('',*,*,#7815,.F.);
#10626=ORIENTED_EDGE('',*,*,#7816,.F.);
#10627=ORIENTED_EDGE('',*,*,#7817,.F.);
#10628=ORIENTED_EDGE('',*,*,#7818,.T.);
#10629=ORIENTED_EDGE('',*,*,#7819,.F.);
#10630=ORIENTED_EDGE('',*,*,#7820,.F.);
#10631=ORIENTED_EDGE('',*,*,#7818,.F.);
#10632=ORIENTED_EDGE('',*,*,#7821,.F.);
#10633=ORIENTED_EDGE('',*,*,#7822,.T.);
#10634=ORIENTED_EDGE('',*,*,#7823,.F.);
#10635=ORIENTED_EDGE('',*,*,#7824,.F.);
#10636=ORIENTED_EDGE('',*,*,#7825,.F.);
#10637=ORIENTED_EDGE('',*,*,#7826,.T.);
#10638=ORIENTED_EDGE('',*,*,#7827,.F.);
#10639=ORIENTED_EDGE('',*,*,#7828,.F.);
#10640=ORIENTED_EDGE('',*,*,#7829,.F.);
#10641=ORIENTED_EDGE('',*,*,#7830,.F.);
#10642=ORIENTED_EDGE('',*,*,#7831,.F.);
#10643=ORIENTED_EDGE('',*,*,#7822,.F.);
#10644=ORIENTED_EDGE('',*,*,#7832,.F.);
#10645=ORIENTED_EDGE('',*,*,#7833,.F.);
#10646=ORIENTED_EDGE('',*,*,#7834,.F.);
#10647=ORIENTED_EDGE('',*,*,#7826,.F.);
#10648=ORIENTED_EDGE('',*,*,#7823,.T.);
#10649=ORIENTED_EDGE('',*,*,#7831,.T.);
#10650=ORIENTED_EDGE('',*,*,#7835,.T.);
#10651=ORIENTED_EDGE('',*,*,#7827,.T.);
#10652=ORIENTED_EDGE('',*,*,#7834,.T.);
#10653=ORIENTED_EDGE('',*,*,#7836,.T.);
#10654=ORIENTED_EDGE('',*,*,#7824,.T.);
#10655=ORIENTED_EDGE('',*,*,#7836,.F.);
#10656=ORIENTED_EDGE('',*,*,#7833,.T.);
#10657=ORIENTED_EDGE('',*,*,#7837,.T.);
#10658=ORIENTED_EDGE('',*,*,#7819,.T.);
#10659=ORIENTED_EDGE('',*,*,#7820,.T.);
#10660=ORIENTED_EDGE('',*,*,#7830,.T.);
#10661=ORIENTED_EDGE('',*,*,#7838,.T.);
#10662=ORIENTED_EDGE('',*,*,#7828,.T.);
#10663=ORIENTED_EDGE('',*,*,#7835,.F.);
#10664=ORIENTED_EDGE('',*,*,#7816,.T.);
#10665=ORIENTED_EDGE('',*,*,#7817,.T.);
#10666=ORIENTED_EDGE('',*,*,#7821,.T.);
#10667=ORIENTED_EDGE('',*,*,#7837,.F.);
#10668=ORIENTED_EDGE('',*,*,#7832,.T.);
#10669=ORIENTED_EDGE('',*,*,#7825,.T.);
#10670=ORIENTED_EDGE('',*,*,#7838,.F.);
#10671=ORIENTED_EDGE('',*,*,#7829,.T.);
#10672=ORIENTED_EDGE('',*,*,#7839,.F.);
#10673=ORIENTED_EDGE('',*,*,#7840,.T.);
#10674=ORIENTED_EDGE('',*,*,#7841,.T.);
#10675=ORIENTED_EDGE('',*,*,#7842,.F.);
#10676=ORIENTED_EDGE('',*,*,#7843,.F.);
#10677=ORIENTED_EDGE('',*,*,#7844,.T.);
#10678=ORIENTED_EDGE('',*,*,#7845,.T.);
#10679=ORIENTED_EDGE('',*,*,#7840,.F.);
#10680=ORIENTED_EDGE('',*,*,#7846,.F.);
#10681=ORIENTED_EDGE('',*,*,#7847,.T.);
#10682=ORIENTED_EDGE('',*,*,#7848,.T.);
#10683=ORIENTED_EDGE('',*,*,#7844,.F.);
#10684=ORIENTED_EDGE('',*,*,#7849,.F.);
#10685=ORIENTED_EDGE('',*,*,#7850,.T.);
#10686=ORIENTED_EDGE('',*,*,#7851,.T.);
#10687=ORIENTED_EDGE('',*,*,#7847,.F.);
#10688=ORIENTED_EDGE('',*,*,#7852,.F.);
#10689=ORIENTED_EDGE('',*,*,#7853,.T.);
#10690=ORIENTED_EDGE('',*,*,#7854,.T.);
#10691=ORIENTED_EDGE('',*,*,#7850,.F.);
#10692=ORIENTED_EDGE('',*,*,#7855,.F.);
#10693=ORIENTED_EDGE('',*,*,#7842,.T.);
#10694=ORIENTED_EDGE('',*,*,#7856,.T.);
#10695=ORIENTED_EDGE('',*,*,#7853,.F.);
#10696=ORIENTED_EDGE('',*,*,#7856,.F.);
#10697=ORIENTED_EDGE('',*,*,#7841,.F.);
#10698=ORIENTED_EDGE('',*,*,#7845,.F.);
#10699=ORIENTED_EDGE('',*,*,#7848,.F.);
#10700=ORIENTED_EDGE('',*,*,#7851,.F.);
#10701=ORIENTED_EDGE('',*,*,#7854,.F.);
#10702=ORIENTED_EDGE('',*,*,#7857,.F.);
#10703=ORIENTED_EDGE('',*,*,#7839,.T.);
#10704=ORIENTED_EDGE('',*,*,#7855,.T.);
#10705=ORIENTED_EDGE('',*,*,#7852,.T.);
#10706=ORIENTED_EDGE('',*,*,#7849,.T.);
#10707=ORIENTED_EDGE('',*,*,#7846,.T.);
#10708=ORIENTED_EDGE('',*,*,#7843,.T.);
#10709=ORIENTED_EDGE('',*,*,#7858,.F.);
#10710=ORIENTED_EDGE('',*,*,#7859,.T.);
#10711=ORIENTED_EDGE('',*,*,#7857,.T.);
#10712=ORIENTED_EDGE('',*,*,#7859,.F.);
#10713=ORIENTED_EDGE('',*,*,#7860,.F.);
#10714=ORIENTED_EDGE('',*,*,#7861,.T.);
#10715=ORIENTED_EDGE('',*,*,#7858,.T.);
#10716=ORIENTED_EDGE('',*,*,#7861,.F.);
#10717=ORIENTED_EDGE('',*,*,#7862,.F.);
#10718=ORIENTED_EDGE('',*,*,#7863,.T.);
#10719=ORIENTED_EDGE('',*,*,#7860,.T.);
#10720=ORIENTED_EDGE('',*,*,#7863,.F.);
#10721=ORIENTED_EDGE('',*,*,#7862,.T.);
#10722=ORIENTED_EDGE('',*,*,#7864,.F.);
#10723=ORIENTED_EDGE('',*,*,#7865,.T.);
#10724=ORIENTED_EDGE('',*,*,#7866,.F.);
#10725=ORIENTED_EDGE('',*,*,#7865,.F.);
#10726=ORIENTED_EDGE('',*,*,#7864,.T.);
#10727=ORIENTED_EDGE('',*,*,#7867,.F.);
#10728=ORIENTED_EDGE('',*,*,#7868,.T.);
#10729=ORIENTED_EDGE('',*,*,#7869,.T.);
#10730=ORIENTED_EDGE('',*,*,#7868,.F.);
#10731=ORIENTED_EDGE('',*,*,#7869,.F.);
#10732=ORIENTED_EDGE('',*,*,#7870,.F.);
#10733=ORIENTED_EDGE('',*,*,#7871,.T.);
#10734=ORIENTED_EDGE('',*,*,#7872,.F.);
#10735=ORIENTED_EDGE('',*,*,#7873,.T.);
#10736=ORIENTED_EDGE('',*,*,#7874,.F.);
#10737=ORIENTED_EDGE('',*,*,#7873,.F.);
#10738=ORIENTED_EDGE('',*,*,#7875,.F.);
#10739=ORIENTED_EDGE('',*,*,#7876,.F.);
#10740=ORIENTED_EDGE('',*,*,#7875,.T.);
#10741=ORIENTED_EDGE('',*,*,#7872,.T.);
#10742=ORIENTED_EDGE('',*,*,#7877,.T.);
#10743=ORIENTED_EDGE('',*,*,#7878,.F.);
#10744=ORIENTED_EDGE('',*,*,#7879,.F.);
#10745=ORIENTED_EDGE('',*,*,#7876,.T.);
#10746=ORIENTED_EDGE('',*,*,#7878,.T.);
#10747=ORIENTED_EDGE('',*,*,#7880,.T.);
#10748=ORIENTED_EDGE('',*,*,#7881,.F.);
#10749=ORIENTED_EDGE('',*,*,#7880,.F.);
#10750=ORIENTED_EDGE('',*,*,#7877,.F.);
#10751=ORIENTED_EDGE('',*,*,#7871,.F.);
#10752=ORIENTED_EDGE('',*,*,#7882,.F.);
#10753=ORIENTED_EDGE('',*,*,#7883,.T.);
#10754=ORIENTED_EDGE('',*,*,#7884,.F.);
#10755=ORIENTED_EDGE('',*,*,#7885,.T.);
#10756=ORIENTED_EDGE('',*,*,#7886,.F.);
#10757=ORIENTED_EDGE('',*,*,#7885,.F.);
#10758=ORIENTED_EDGE('',*,*,#7887,.F.);
#10759=ORIENTED_EDGE('',*,*,#7888,.F.);
#10760=ORIENTED_EDGE('',*,*,#7887,.T.);
#10761=ORIENTED_EDGE('',*,*,#7884,.T.);
#10762=ORIENTED_EDGE('',*,*,#7889,.T.);
#10763=ORIENTED_EDGE('',*,*,#7890,.F.);
#10764=ORIENTED_EDGE('',*,*,#7891,.F.);
#10765=ORIENTED_EDGE('',*,*,#7888,.T.);
#10766=ORIENTED_EDGE('',*,*,#7890,.T.);
#10767=ORIENTED_EDGE('',*,*,#7892,.T.);
#10768=ORIENTED_EDGE('',*,*,#7893,.F.);
#10769=ORIENTED_EDGE('',*,*,#7892,.F.);
#10770=ORIENTED_EDGE('',*,*,#7889,.F.);
#10771=ORIENTED_EDGE('',*,*,#7883,.F.);
#10772=ORIENTED_EDGE('',*,*,#7894,.F.);
#10773=ORIENTED_EDGE('',*,*,#7895,.T.);
#10774=ORIENTED_EDGE('',*,*,#7896,.T.);
#10775=ORIENTED_EDGE('',*,*,#7895,.F.);
#10776=ORIENTED_EDGE('',*,*,#7879,.T.);
#10777=ORIENTED_EDGE('',*,*,#7881,.T.);
#10778=ORIENTED_EDGE('',*,*,#7870,.T.);
#10779=ORIENTED_EDGE('',*,*,#7874,.T.);
#10780=ORIENTED_EDGE('',*,*,#7891,.T.);
#10781=ORIENTED_EDGE('',*,*,#7893,.T.);
#10782=ORIENTED_EDGE('',*,*,#7882,.T.);
#10783=ORIENTED_EDGE('',*,*,#7886,.T.);
#10784=ORIENTED_EDGE('',*,*,#7894,.T.);
#10785=ORIENTED_EDGE('',*,*,#7866,.T.);
#10786=ORIENTED_EDGE('',*,*,#7896,.F.);
#10787=ORIENTED_EDGE('',*,*,#7867,.T.);
#10788=ORIENTED_EDGE('',*,*,#7897,.F.);
#10789=ORIENTED_EDGE('',*,*,#7898,.T.);
#10790=ORIENTED_EDGE('',*,*,#7899,.T.);
#10791=ORIENTED_EDGE('',*,*,#7898,.F.);
#10792=ORIENTED_EDGE('',*,*,#7900,.F.);
#10793=ORIENTED_EDGE('',*,*,#7901,.T.);
#10794=ORIENTED_EDGE('',*,*,#7902,.T.);
#10795=ORIENTED_EDGE('',*,*,#7901,.F.);
#10796=ORIENTED_EDGE('',*,*,#7900,.T.);
#10797=ORIENTED_EDGE('',*,*,#7897,.T.);
#10798=ORIENTED_EDGE('',*,*,#7902,.F.);
#10799=ORIENTED_EDGE('',*,*,#7899,.F.);
#10800=ORIENTED_EDGE('',*,*,#7903,.F.);
#10801=ORIENTED_EDGE('',*,*,#7904,.T.);
#10802=ORIENTED_EDGE('',*,*,#7905,.T.);
#10803=ORIENTED_EDGE('',*,*,#7904,.F.);
#10804=ORIENTED_EDGE('',*,*,#7906,.F.);
#10805=ORIENTED_EDGE('',*,*,#7907,.T.);
#10806=ORIENTED_EDGE('',*,*,#7908,.T.);
#10807=ORIENTED_EDGE('',*,*,#7907,.F.);
#10808=ORIENTED_EDGE('',*,*,#7906,.T.);
#10809=ORIENTED_EDGE('',*,*,#7903,.T.);
#10810=ORIENTED_EDGE('',*,*,#7908,.F.);
#10811=ORIENTED_EDGE('',*,*,#7905,.F.);
#10812=ORIENTED_EDGE('',*,*,#7909,.F.);
#10813=ORIENTED_EDGE('',*,*,#7910,.T.);
#10814=ORIENTED_EDGE('',*,*,#7911,.T.);
#10815=ORIENTED_EDGE('',*,*,#7910,.F.);
#10816=ORIENTED_EDGE('',*,*,#7912,.F.);
#10817=ORIENTED_EDGE('',*,*,#7913,.T.);
#10818=ORIENTED_EDGE('',*,*,#7914,.T.);
#10819=ORIENTED_EDGE('',*,*,#7913,.F.);
#10820=ORIENTED_EDGE('',*,*,#7912,.T.);
#10821=ORIENTED_EDGE('',*,*,#7909,.T.);
#10822=ORIENTED_EDGE('',*,*,#7914,.F.);
#10823=ORIENTED_EDGE('',*,*,#7911,.F.);
#10824=ORIENTED_EDGE('',*,*,#7915,.F.);
#10825=ORIENTED_EDGE('',*,*,#7916,.T.);
#10826=ORIENTED_EDGE('',*,*,#7917,.T.);
#10827=ORIENTED_EDGE('',*,*,#7916,.F.);
#10828=ORIENTED_EDGE('',*,*,#7918,.F.);
#10829=ORIENTED_EDGE('',*,*,#7919,.T.);
#10830=ORIENTED_EDGE('',*,*,#7920,.T.);
#10831=ORIENTED_EDGE('',*,*,#7919,.F.);
#10832=ORIENTED_EDGE('',*,*,#7918,.T.);
#10833=ORIENTED_EDGE('',*,*,#7915,.T.);
#10834=ORIENTED_EDGE('',*,*,#7920,.F.);
#10835=ORIENTED_EDGE('',*,*,#7917,.F.);
#10836=ORIENTED_EDGE('',*,*,#7921,.T.);
#10837=ORIENTED_EDGE('',*,*,#7922,.T.);
#10838=ORIENTED_EDGE('',*,*,#7923,.F.);
#10839=ORIENTED_EDGE('',*,*,#7924,.F.);
#10840=ORIENTED_EDGE('',*,*,#7925,.T.);
#10841=ORIENTED_EDGE('',*,*,#7924,.T.);
#10842=ORIENTED_EDGE('',*,*,#7926,.F.);
#10843=ORIENTED_EDGE('',*,*,#7927,.F.);
#10844=ORIENTED_EDGE('',*,*,#7928,.T.);
#10845=ORIENTED_EDGE('',*,*,#7927,.T.);
#10846=ORIENTED_EDGE('',*,*,#7929,.F.);
#10847=ORIENTED_EDGE('',*,*,#7930,.F.);
#10848=ORIENTED_EDGE('',*,*,#7931,.T.);
#10849=ORIENTED_EDGE('',*,*,#7930,.T.);
#10850=ORIENTED_EDGE('',*,*,#7932,.F.);
#10851=ORIENTED_EDGE('',*,*,#7922,.F.);
#10852=ORIENTED_EDGE('',*,*,#7932,.T.);
#10853=ORIENTED_EDGE('',*,*,#7929,.T.);
#10854=ORIENTED_EDGE('',*,*,#7926,.T.);
#10855=ORIENTED_EDGE('',*,*,#7923,.T.);
#10856=ORIENTED_EDGE('',*,*,#7931,.F.);
#10857=ORIENTED_EDGE('',*,*,#7921,.F.);
#10858=ORIENTED_EDGE('',*,*,#7925,.F.);
#10859=ORIENTED_EDGE('',*,*,#7928,.F.);
#10860=ORIENTED_EDGE('',*,*,#7933,.T.);
#10861=ORIENTED_EDGE('',*,*,#7934,.T.);
#10862=ORIENTED_EDGE('',*,*,#7935,.F.);
#10863=ORIENTED_EDGE('',*,*,#7936,.F.);
#10864=ORIENTED_EDGE('',*,*,#7937,.T.);
#10865=ORIENTED_EDGE('',*,*,#7936,.T.);
#10866=ORIENTED_EDGE('',*,*,#7938,.F.);
#10867=ORIENTED_EDGE('',*,*,#7939,.F.);
#10868=ORIENTED_EDGE('',*,*,#7940,.T.);
#10869=ORIENTED_EDGE('',*,*,#7939,.T.);
#10870=ORIENTED_EDGE('',*,*,#7941,.F.);
#10871=ORIENTED_EDGE('',*,*,#7942,.F.);
#10872=ORIENTED_EDGE('',*,*,#7943,.T.);
#10873=ORIENTED_EDGE('',*,*,#7942,.T.);
#10874=ORIENTED_EDGE('',*,*,#7944,.F.);
#10875=ORIENTED_EDGE('',*,*,#7934,.F.);
#10876=ORIENTED_EDGE('',*,*,#7944,.T.);
#10877=ORIENTED_EDGE('',*,*,#7941,.T.);
#10878=ORIENTED_EDGE('',*,*,#7938,.T.);
#10879=ORIENTED_EDGE('',*,*,#7935,.T.);
#10880=ORIENTED_EDGE('',*,*,#7943,.F.);
#10881=ORIENTED_EDGE('',*,*,#7933,.F.);
#10882=ORIENTED_EDGE('',*,*,#7937,.F.);
#10883=ORIENTED_EDGE('',*,*,#7940,.F.);
#10884=ORIENTED_EDGE('',*,*,#7945,.F.);
#10885=ORIENTED_EDGE('',*,*,#7946,.T.);
#10886=ORIENTED_EDGE('',*,*,#7947,.F.);
#10887=ORIENTED_EDGE('',*,*,#7946,.F.);
#10888=ORIENTED_EDGE('',*,*,#7948,.F.);
#10889=ORIENTED_EDGE('',*,*,#7949,.T.);
#10890=ORIENTED_EDGE('',*,*,#7950,.F.);
#10891=ORIENTED_EDGE('',*,*,#7951,.F.);
#10892=ORIENTED_EDGE('',*,*,#7952,.F.);
#10893=ORIENTED_EDGE('',*,*,#7953,.T.);
#10894=ORIENTED_EDGE('',*,*,#7954,.F.);
#10895=ORIENTED_EDGE('',*,*,#7949,.F.);
#10896=ORIENTED_EDGE('',*,*,#7955,.F.);
#10897=ORIENTED_EDGE('',*,*,#7956,.F.);
#10898=ORIENTED_EDGE('',*,*,#7957,.F.);
#10899=ORIENTED_EDGE('',*,*,#7953,.F.);
#10900=ORIENTED_EDGE('',*,*,#7958,.T.);
#10901=ORIENTED_EDGE('',*,*,#7950,.T.);
#10902=ORIENTED_EDGE('',*,*,#7954,.T.);
#10903=ORIENTED_EDGE('',*,*,#7957,.T.);
#10904=ORIENTED_EDGE('',*,*,#7959,.T.);
#10905=ORIENTED_EDGE('',*,*,#7951,.T.);
#10906=ORIENTED_EDGE('',*,*,#7959,.F.);
#10907=ORIENTED_EDGE('',*,*,#7956,.T.);
#10908=ORIENTED_EDGE('',*,*,#7960,.T.);
#10909=ORIENTED_EDGE('',*,*,#7961,.F.);
#10910=ORIENTED_EDGE('',*,*,#7962,.F.);
#10911=ORIENTED_EDGE('',*,*,#7963,.F.);
#10912=ORIENTED_EDGE('',*,*,#7964,.T.);
#10913=ORIENTED_EDGE('',*,*,#7961,.T.);
#10914=ORIENTED_EDGE('',*,*,#7965,.F.);
#10915=ORIENTED_EDGE('',*,*,#7966,.F.);
#10916=ORIENTED_EDGE('',*,*,#7967,.F.);
#10917=ORIENTED_EDGE('',*,*,#7964,.F.);
#10918=ORIENTED_EDGE('',*,*,#7968,.T.);
#10919=ORIENTED_EDGE('',*,*,#7969,.F.);
#10920=ORIENTED_EDGE('',*,*,#7965,.T.);
#10921=ORIENTED_EDGE('',*,*,#7945,.T.);
#10922=ORIENTED_EDGE('',*,*,#7963,.T.);
#10923=ORIENTED_EDGE('',*,*,#7970,.F.);
#10924=ORIENTED_EDGE('',*,*,#7971,.F.);
#10925=ORIENTED_EDGE('',*,*,#7968,.F.);
#10926=ORIENTED_EDGE('',*,*,#7967,.T.);
#10927=ORIENTED_EDGE('',*,*,#7972,.F.);
#10928=ORIENTED_EDGE('',*,*,#7970,.T.);
#10929=ORIENTED_EDGE('',*,*,#7962,.T.);
#10930=ORIENTED_EDGE('',*,*,#7947,.T.);
#10931=ORIENTED_EDGE('',*,*,#7958,.F.);
#10932=ORIENTED_EDGE('',*,*,#7973,.T.);
#10933=ORIENTED_EDGE('',*,*,#7974,.T.);
#10934=ORIENTED_EDGE('',*,*,#7973,.F.);
#10935=ORIENTED_EDGE('',*,*,#7966,.T.);
#10936=ORIENTED_EDGE('',*,*,#7969,.T.);
#10937=ORIENTED_EDGE('',*,*,#7971,.T.);
#10938=ORIENTED_EDGE('',*,*,#7972,.T.);
#10939=ORIENTED_EDGE('',*,*,#7974,.F.);
#10940=ORIENTED_EDGE('',*,*,#7948,.T.);
#10941=ORIENTED_EDGE('',*,*,#7960,.F.);
#10942=ORIENTED_EDGE('',*,*,#7955,.T.);
#10943=ORIENTED_EDGE('',*,*,#7952,.T.);
#10944=ORIENTED_EDGE('',*,*,#7975,.F.);
#10945=ORIENTED_EDGE('',*,*,#7976,.T.);
#10946=ORIENTED_EDGE('',*,*,#7977,.T.);
#10947=ORIENTED_EDGE('',*,*,#7976,.F.);
#10948=ORIENTED_EDGE('',*,*,#7978,.F.);
#10949=ORIENTED_EDGE('',*,*,#7979,.T.);
#10950=ORIENTED_EDGE('',*,*,#7980,.T.);
#10951=ORIENTED_EDGE('',*,*,#7979,.F.);
#10952=ORIENTED_EDGE('',*,*,#7978,.T.);
#10953=ORIENTED_EDGE('',*,*,#7975,.T.);
#10954=ORIENTED_EDGE('',*,*,#7980,.F.);
#10955=ORIENTED_EDGE('',*,*,#7977,.F.);
#10956=ORIENTED_EDGE('',*,*,#7981,.F.);
#10957=ORIENTED_EDGE('',*,*,#7982,.T.);
#10958=ORIENTED_EDGE('',*,*,#7983,.T.);
#10959=ORIENTED_EDGE('',*,*,#7982,.F.);
#10960=ORIENTED_EDGE('',*,*,#7984,.F.);
#10961=ORIENTED_EDGE('',*,*,#7985,.T.);
#10962=ORIENTED_EDGE('',*,*,#7986,.T.);
#10963=ORIENTED_EDGE('',*,*,#7985,.F.);
#10964=ORIENTED_EDGE('',*,*,#7984,.T.);
#10965=ORIENTED_EDGE('',*,*,#7981,.T.);
#10966=ORIENTED_EDGE('',*,*,#7986,.F.);
#10967=ORIENTED_EDGE('',*,*,#7983,.F.);
#10968=ORIENTED_EDGE('',*,*,#7987,.F.);
#10969=ORIENTED_EDGE('',*,*,#7988,.T.);
#10970=ORIENTED_EDGE('',*,*,#7989,.T.);
#10971=ORIENTED_EDGE('',*,*,#7988,.F.);
#10972=ORIENTED_EDGE('',*,*,#7990,.F.);
#10973=ORIENTED_EDGE('',*,*,#7991,.T.);
#10974=ORIENTED_EDGE('',*,*,#7992,.T.);
#10975=ORIENTED_EDGE('',*,*,#7991,.F.);
#10976=ORIENTED_EDGE('',*,*,#7990,.T.);
#10977=ORIENTED_EDGE('',*,*,#7987,.T.);
#10978=ORIENTED_EDGE('',*,*,#7992,.F.);
#10979=ORIENTED_EDGE('',*,*,#7989,.F.);
#10980=ORIENTED_EDGE('',*,*,#7993,.F.);
#10981=ORIENTED_EDGE('',*,*,#7994,.F.);
#10982=ORIENTED_EDGE('',*,*,#7995,.F.);
#10983=ORIENTED_EDGE('',*,*,#7996,.F.);
#10984=ORIENTED_EDGE('',*,*,#7997,.F.);
#10985=ORIENTED_EDGE('',*,*,#7998,.T.);
#10986=ORIENTED_EDGE('',*,*,#7999,.F.);
#10987=ORIENTED_EDGE('',*,*,#7994,.T.);
#10988=ORIENTED_EDGE('',*,*,#8000,.F.);
#10989=ORIENTED_EDGE('',*,*,#8001,.F.);
#10990=ORIENTED_EDGE('',*,*,#8002,.F.);
#10991=ORIENTED_EDGE('',*,*,#7998,.F.);
#10992=ORIENTED_EDGE('',*,*,#8003,.T.);
#10993=ORIENTED_EDGE('',*,*,#8004,.T.);
#10994=ORIENTED_EDGE('',*,*,#8005,.T.);
#10995=ORIENTED_EDGE('',*,*,#8006,.T.);
#10996=ORIENTED_EDGE('',*,*,#8007,.T.);
#10997=ORIENTED_EDGE('',*,*,#8008,.T.);
#10998=ORIENTED_EDGE('',*,*,#8009,.T.);
#10999=ORIENTED_EDGE('',*,*,#8010,.T.);
#11000=ORIENTED_EDGE('',*,*,#8011,.T.);
#11001=ORIENTED_EDGE('',*,*,#8012,.T.);
#11002=ORIENTED_EDGE('',*,*,#8013,.T.);
#11003=ORIENTED_EDGE('',*,*,#8014,.T.);
#11004=ORIENTED_EDGE('',*,*,#8015,.T.);
#11005=ORIENTED_EDGE('',*,*,#8016,.T.);
#11006=ORIENTED_EDGE('',*,*,#8017,.T.);
#11007=ORIENTED_EDGE('',*,*,#8018,.T.);
#11008=ORIENTED_EDGE('',*,*,#8019,.T.);
#11009=ORIENTED_EDGE('',*,*,#8020,.T.);
#11010=ORIENTED_EDGE('',*,*,#8021,.T.);
#11011=ORIENTED_EDGE('',*,*,#8022,.T.);
#11012=ORIENTED_EDGE('',*,*,#8023,.T.);
#11013=ORIENTED_EDGE('',*,*,#8024,.T.);
#11014=ORIENTED_EDGE('',*,*,#8025,.T.);
#11015=ORIENTED_EDGE('',*,*,#8026,.T.);
#11016=ORIENTED_EDGE('',*,*,#8027,.T.);
#11017=ORIENTED_EDGE('',*,*,#8028,.T.);
#11018=ORIENTED_EDGE('',*,*,#8029,.T.);
#11019=ORIENTED_EDGE('',*,*,#8030,.T.);
#11020=ORIENTED_EDGE('',*,*,#8031,.T.);
#11021=ORIENTED_EDGE('',*,*,#8032,.T.);
#11022=ORIENTED_EDGE('',*,*,#8033,.T.);
#11023=ORIENTED_EDGE('',*,*,#8034,.T.);
#11024=ORIENTED_EDGE('',*,*,#8035,.T.);
#11025=ORIENTED_EDGE('',*,*,#8036,.T.);
#11026=ORIENTED_EDGE('',*,*,#8037,.T.);
#11027=ORIENTED_EDGE('',*,*,#8038,.T.);
#11028=ORIENTED_EDGE('',*,*,#8039,.T.);
#11029=ORIENTED_EDGE('',*,*,#8040,.T.);
#11030=ORIENTED_EDGE('',*,*,#8041,.T.);
#11031=ORIENTED_EDGE('',*,*,#8042,.T.);
#11032=ORIENTED_EDGE('',*,*,#8043,.T.);
#11033=ORIENTED_EDGE('',*,*,#8044,.T.);
#11034=ORIENTED_EDGE('',*,*,#8045,.T.);
#11035=ORIENTED_EDGE('',*,*,#8046,.T.);
#11036=ORIENTED_EDGE('',*,*,#8047,.T.);
#11037=ORIENTED_EDGE('',*,*,#8048,.T.);
#11038=ORIENTED_EDGE('',*,*,#8049,.T.);
#11039=ORIENTED_EDGE('',*,*,#8050,.T.);
#11040=ORIENTED_EDGE('',*,*,#8051,.T.);
#11041=ORIENTED_EDGE('',*,*,#8052,.T.);
#11042=ORIENTED_EDGE('',*,*,#8053,.T.);
#11043=ORIENTED_EDGE('',*,*,#8054,.T.);
#11044=ORIENTED_EDGE('',*,*,#8055,.T.);
#11045=ORIENTED_EDGE('',*,*,#8056,.T.);
#11046=ORIENTED_EDGE('',*,*,#8057,.T.);
#11047=ORIENTED_EDGE('',*,*,#8058,.T.);
#11048=ORIENTED_EDGE('',*,*,#8059,.T.);
#11049=ORIENTED_EDGE('',*,*,#8060,.T.);
#11050=ORIENTED_EDGE('',*,*,#8061,.T.);
#11051=ORIENTED_EDGE('',*,*,#8062,.T.);
#11052=ORIENTED_EDGE('',*,*,#8063,.T.);
#11053=ORIENTED_EDGE('',*,*,#8064,.T.);
#11054=ORIENTED_EDGE('',*,*,#8065,.T.);
#11055=ORIENTED_EDGE('',*,*,#8066,.T.);
#11056=ORIENTED_EDGE('',*,*,#8067,.T.);
#11057=ORIENTED_EDGE('',*,*,#8068,.T.);
#11058=ORIENTED_EDGE('',*,*,#8069,.T.);
#11059=ORIENTED_EDGE('',*,*,#8070,.T.);
#11060=ORIENTED_EDGE('',*,*,#8071,.T.);
#11061=ORIENTED_EDGE('',*,*,#8072,.T.);
#11062=ORIENTED_EDGE('',*,*,#8073,.T.);
#11063=ORIENTED_EDGE('',*,*,#8074,.T.);
#11064=ORIENTED_EDGE('',*,*,#8075,.T.);
#11065=ORIENTED_EDGE('',*,*,#8076,.T.);
#11066=ORIENTED_EDGE('',*,*,#8077,.T.);
#11067=ORIENTED_EDGE('',*,*,#8078,.T.);
#11068=ORIENTED_EDGE('',*,*,#8079,.T.);
#11069=ORIENTED_EDGE('',*,*,#8080,.T.);
#11070=ORIENTED_EDGE('',*,*,#8081,.T.);
#11071=ORIENTED_EDGE('',*,*,#8082,.T.);
#11072=ORIENTED_EDGE('',*,*,#7995,.T.);
#11073=ORIENTED_EDGE('',*,*,#7999,.T.);
#11074=ORIENTED_EDGE('',*,*,#8002,.T.);
#11075=ORIENTED_EDGE('',*,*,#8083,.T.);
#11076=ORIENTED_EDGE('',*,*,#7996,.T.);
#11077=ORIENTED_EDGE('',*,*,#8083,.F.);
#11078=ORIENTED_EDGE('',*,*,#8001,.T.);
#11079=ORIENTED_EDGE('',*,*,#8084,.F.);
#11080=ORIENTED_EDGE('',*,*,#8085,.F.);
#11081=ORIENTED_EDGE('',*,*,#8086,.T.);
#11082=ORIENTED_EDGE('',*,*,#8087,.F.);
#11083=ORIENTED_EDGE('',*,*,#8086,.F.);
#11084=ORIENTED_EDGE('',*,*,#8085,.T.);
#11085=ORIENTED_EDGE('',*,*,#7993,.T.);
#11086=ORIENTED_EDGE('',*,*,#8084,.T.);
#11087=ORIENTED_EDGE('',*,*,#8000,.T.);
#11088=ORIENTED_EDGE('',*,*,#7997,.T.);
#11089=ORIENTED_EDGE('',*,*,#8088,.F.);
#11090=ORIENTED_EDGE('',*,*,#8089,.F.);
#11091=ORIENTED_EDGE('',*,*,#8090,.F.);
#11092=ORIENTED_EDGE('',*,*,#8080,.F.);
#11093=ORIENTED_EDGE('',*,*,#8090,.T.);
#11094=ORIENTED_EDGE('',*,*,#8091,.F.);
#11095=ORIENTED_EDGE('',*,*,#8092,.F.);
#11096=ORIENTED_EDGE('',*,*,#8081,.F.);
#11097=ORIENTED_EDGE('',*,*,#8092,.T.);
#11098=ORIENTED_EDGE('',*,*,#8093,.F.);
#11099=ORIENTED_EDGE('',*,*,#8094,.F.);
#11100=ORIENTED_EDGE('',*,*,#8082,.F.);
#11101=ORIENTED_EDGE('',*,*,#8094,.T.);
#11102=ORIENTED_EDGE('',*,*,#8095,.F.);
#11103=ORIENTED_EDGE('',*,*,#8096,.T.);
#11104=ORIENTED_EDGE('',*,*,#8003,.F.);
#11105=ORIENTED_EDGE('',*,*,#8096,.F.);
#11106=ORIENTED_EDGE('',*,*,#8097,.F.);
#11107=ORIENTED_EDGE('',*,*,#8098,.F.);
#11108=ORIENTED_EDGE('',*,*,#8004,.F.);
#11109=ORIENTED_EDGE('',*,*,#8098,.T.);
#11110=ORIENTED_EDGE('',*,*,#8099,.F.);
#11111=ORIENTED_EDGE('',*,*,#8100,.F.);
#11112=ORIENTED_EDGE('',*,*,#8005,.F.);
#11113=ORIENTED_EDGE('',*,*,#8100,.T.);
#11114=ORIENTED_EDGE('',*,*,#8101,.F.);
#11115=ORIENTED_EDGE('',*,*,#8102,.F.);
#11116=ORIENTED_EDGE('',*,*,#8006,.F.);
#11117=ORIENTED_EDGE('',*,*,#8102,.T.);
#11118=ORIENTED_EDGE('',*,*,#8103,.F.);
#11119=ORIENTED_EDGE('',*,*,#8104,.T.);
#11120=ORIENTED_EDGE('',*,*,#8007,.F.);
#11121=ORIENTED_EDGE('',*,*,#8104,.F.);
#11122=ORIENTED_EDGE('',*,*,#8105,.F.);
#11123=ORIENTED_EDGE('',*,*,#8106,.F.);
#11124=ORIENTED_EDGE('',*,*,#8008,.F.);
#11125=ORIENTED_EDGE('',*,*,#8106,.T.);
#11126=ORIENTED_EDGE('',*,*,#8107,.F.);
#11127=ORIENTED_EDGE('',*,*,#8108,.F.);
#11128=ORIENTED_EDGE('',*,*,#8009,.F.);
#11129=ORIENTED_EDGE('',*,*,#8108,.T.);
#11130=ORIENTED_EDGE('',*,*,#8109,.F.);
#11131=ORIENTED_EDGE('',*,*,#8110,.F.);
#11132=ORIENTED_EDGE('',*,*,#8010,.F.);
#11133=ORIENTED_EDGE('',*,*,#8110,.T.);
#11134=ORIENTED_EDGE('',*,*,#8111,.F.);
#11135=ORIENTED_EDGE('',*,*,#8112,.T.);
#11136=ORIENTED_EDGE('',*,*,#8011,.F.);
#11137=ORIENTED_EDGE('',*,*,#8112,.F.);
#11138=ORIENTED_EDGE('',*,*,#8113,.F.);
#11139=ORIENTED_EDGE('',*,*,#8114,.F.);
#11140=ORIENTED_EDGE('',*,*,#8012,.F.);
#11141=ORIENTED_EDGE('',*,*,#8114,.T.);
#11142=ORIENTED_EDGE('',*,*,#8115,.F.);
#11143=ORIENTED_EDGE('',*,*,#8116,.F.);
#11144=ORIENTED_EDGE('',*,*,#8013,.F.);
#11145=ORIENTED_EDGE('',*,*,#8116,.T.);
#11146=ORIENTED_EDGE('',*,*,#8117,.F.);
#11147=ORIENTED_EDGE('',*,*,#8118,.F.);
#11148=ORIENTED_EDGE('',*,*,#8014,.F.);
#11149=ORIENTED_EDGE('',*,*,#8118,.T.);
#11150=ORIENTED_EDGE('',*,*,#8119,.F.);
#11151=ORIENTED_EDGE('',*,*,#8120,.T.);
#11152=ORIENTED_EDGE('',*,*,#8015,.F.);
#11153=ORIENTED_EDGE('',*,*,#8120,.F.);
#11154=ORIENTED_EDGE('',*,*,#8121,.F.);
#11155=ORIENTED_EDGE('',*,*,#8122,.F.);
#11156=ORIENTED_EDGE('',*,*,#8016,.F.);
#11157=ORIENTED_EDGE('',*,*,#8122,.T.);
#11158=ORIENTED_EDGE('',*,*,#8123,.F.);
#11159=ORIENTED_EDGE('',*,*,#8124,.F.);
#11160=ORIENTED_EDGE('',*,*,#8017,.F.);
#11161=ORIENTED_EDGE('',*,*,#8124,.T.);
#11162=ORIENTED_EDGE('',*,*,#8125,.F.);
#11163=ORIENTED_EDGE('',*,*,#8126,.F.);
#11164=ORIENTED_EDGE('',*,*,#8018,.F.);
#11165=ORIENTED_EDGE('',*,*,#8126,.T.);
#11166=ORIENTED_EDGE('',*,*,#8127,.F.);
#11167=ORIENTED_EDGE('',*,*,#8128,.T.);
#11168=ORIENTED_EDGE('',*,*,#8019,.F.);
#11169=ORIENTED_EDGE('',*,*,#8128,.F.);
#11170=ORIENTED_EDGE('',*,*,#8129,.F.);
#11171=ORIENTED_EDGE('',*,*,#8130,.F.);
#11172=ORIENTED_EDGE('',*,*,#8020,.F.);
#11173=ORIENTED_EDGE('',*,*,#8130,.T.);
#11174=ORIENTED_EDGE('',*,*,#8131,.F.);
#11175=ORIENTED_EDGE('',*,*,#8132,.F.);
#11176=ORIENTED_EDGE('',*,*,#8021,.F.);
#11177=ORIENTED_EDGE('',*,*,#8132,.T.);
#11178=ORIENTED_EDGE('',*,*,#8133,.F.);
#11179=ORIENTED_EDGE('',*,*,#8134,.F.);
#11180=ORIENTED_EDGE('',*,*,#8022,.F.);
#11181=ORIENTED_EDGE('',*,*,#8134,.T.);
#11182=ORIENTED_EDGE('',*,*,#8135,.F.);
#11183=ORIENTED_EDGE('',*,*,#8136,.T.);
#11184=ORIENTED_EDGE('',*,*,#8023,.F.);
#11185=ORIENTED_EDGE('',*,*,#8136,.F.);
#11186=ORIENTED_EDGE('',*,*,#8137,.F.);
#11187=ORIENTED_EDGE('',*,*,#8138,.F.);
#11188=ORIENTED_EDGE('',*,*,#8024,.F.);
#11189=ORIENTED_EDGE('',*,*,#8138,.T.);
#11190=ORIENTED_EDGE('',*,*,#8139,.F.);
#11191=ORIENTED_EDGE('',*,*,#8140,.F.);
#11192=ORIENTED_EDGE('',*,*,#8025,.F.);
#11193=ORIENTED_EDGE('',*,*,#8140,.T.);
#11194=ORIENTED_EDGE('',*,*,#8141,.F.);
#11195=ORIENTED_EDGE('',*,*,#8142,.F.);
#11196=ORIENTED_EDGE('',*,*,#8026,.F.);
#11197=ORIENTED_EDGE('',*,*,#8142,.T.);
#11198=ORIENTED_EDGE('',*,*,#8143,.F.);
#11199=ORIENTED_EDGE('',*,*,#8144,.T.);
#11200=ORIENTED_EDGE('',*,*,#8027,.F.);
#11201=ORIENTED_EDGE('',*,*,#8144,.F.);
#11202=ORIENTED_EDGE('',*,*,#8145,.F.);
#11203=ORIENTED_EDGE('',*,*,#8146,.F.);
#11204=ORIENTED_EDGE('',*,*,#8028,.F.);
#11205=ORIENTED_EDGE('',*,*,#8146,.T.);
#11206=ORIENTED_EDGE('',*,*,#8147,.F.);
#11207=ORIENTED_EDGE('',*,*,#8148,.F.);
#11208=ORIENTED_EDGE('',*,*,#8029,.F.);
#11209=ORIENTED_EDGE('',*,*,#8148,.T.);
#11210=ORIENTED_EDGE('',*,*,#8149,.F.);
#11211=ORIENTED_EDGE('',*,*,#8150,.F.);
#11212=ORIENTED_EDGE('',*,*,#8030,.F.);
#11213=ORIENTED_EDGE('',*,*,#8150,.T.);
#11214=ORIENTED_EDGE('',*,*,#8151,.F.);
#11215=ORIENTED_EDGE('',*,*,#8152,.T.);
#11216=ORIENTED_EDGE('',*,*,#8031,.F.);
#11217=ORIENTED_EDGE('',*,*,#8152,.F.);
#11218=ORIENTED_EDGE('',*,*,#8153,.F.);
#11219=ORIENTED_EDGE('',*,*,#8154,.F.);
#11220=ORIENTED_EDGE('',*,*,#8032,.F.);
#11221=ORIENTED_EDGE('',*,*,#8154,.T.);
#11222=ORIENTED_EDGE('',*,*,#8155,.F.);
#11223=ORIENTED_EDGE('',*,*,#8156,.F.);
#11224=ORIENTED_EDGE('',*,*,#8033,.F.);
#11225=ORIENTED_EDGE('',*,*,#8156,.T.);
#11226=ORIENTED_EDGE('',*,*,#8157,.F.);
#11227=ORIENTED_EDGE('',*,*,#8158,.F.);
#11228=ORIENTED_EDGE('',*,*,#8034,.F.);
#11229=ORIENTED_EDGE('',*,*,#8158,.T.);
#11230=ORIENTED_EDGE('',*,*,#8159,.F.);
#11231=ORIENTED_EDGE('',*,*,#8160,.T.);
#11232=ORIENTED_EDGE('',*,*,#8035,.F.);
#11233=ORIENTED_EDGE('',*,*,#8160,.F.);
#11234=ORIENTED_EDGE('',*,*,#8161,.F.);
#11235=ORIENTED_EDGE('',*,*,#8162,.F.);
#11236=ORIENTED_EDGE('',*,*,#8036,.F.);
#11237=ORIENTED_EDGE('',*,*,#8162,.T.);
#11238=ORIENTED_EDGE('',*,*,#8163,.F.);
#11239=ORIENTED_EDGE('',*,*,#8164,.F.);
#11240=ORIENTED_EDGE('',*,*,#8037,.F.);
#11241=ORIENTED_EDGE('',*,*,#8164,.T.);
#11242=ORIENTED_EDGE('',*,*,#8165,.F.);
#11243=ORIENTED_EDGE('',*,*,#8166,.F.);
#11244=ORIENTED_EDGE('',*,*,#8038,.F.);
#11245=ORIENTED_EDGE('',*,*,#8166,.T.);
#11246=ORIENTED_EDGE('',*,*,#8167,.F.);
#11247=ORIENTED_EDGE('',*,*,#8168,.T.);
#11248=ORIENTED_EDGE('',*,*,#8039,.F.);
#11249=ORIENTED_EDGE('',*,*,#8168,.F.);
#11250=ORIENTED_EDGE('',*,*,#8169,.F.);
#11251=ORIENTED_EDGE('',*,*,#8170,.F.);
#11252=ORIENTED_EDGE('',*,*,#8040,.F.);
#11253=ORIENTED_EDGE('',*,*,#8170,.T.);
#11254=ORIENTED_EDGE('',*,*,#8171,.F.);
#11255=ORIENTED_EDGE('',*,*,#8172,.F.);
#11256=ORIENTED_EDGE('',*,*,#8041,.F.);
#11257=ORIENTED_EDGE('',*,*,#8172,.T.);
#11258=ORIENTED_EDGE('',*,*,#8173,.F.);
#11259=ORIENTED_EDGE('',*,*,#8174,.F.);
#11260=ORIENTED_EDGE('',*,*,#8042,.F.);
#11261=ORIENTED_EDGE('',*,*,#8174,.T.);
#11262=ORIENTED_EDGE('',*,*,#8175,.F.);
#11263=ORIENTED_EDGE('',*,*,#8176,.T.);
#11264=ORIENTED_EDGE('',*,*,#8043,.F.);
#11265=ORIENTED_EDGE('',*,*,#8176,.F.);
#11266=ORIENTED_EDGE('',*,*,#8177,.F.);
#11267=ORIENTED_EDGE('',*,*,#8178,.F.);
#11268=ORIENTED_EDGE('',*,*,#8044,.F.);
#11269=ORIENTED_EDGE('',*,*,#8178,.T.);
#11270=ORIENTED_EDGE('',*,*,#8179,.F.);
#11271=ORIENTED_EDGE('',*,*,#8180,.F.);
#11272=ORIENTED_EDGE('',*,*,#8045,.F.);
#11273=ORIENTED_EDGE('',*,*,#8180,.T.);
#11274=ORIENTED_EDGE('',*,*,#8181,.F.);
#11275=ORIENTED_EDGE('',*,*,#8182,.F.);
#11276=ORIENTED_EDGE('',*,*,#8046,.F.);
#11277=ORIENTED_EDGE('',*,*,#8182,.T.);
#11278=ORIENTED_EDGE('',*,*,#8183,.F.);
#11279=ORIENTED_EDGE('',*,*,#8184,.T.);
#11280=ORIENTED_EDGE('',*,*,#8047,.F.);
#11281=ORIENTED_EDGE('',*,*,#8184,.F.);
#11282=ORIENTED_EDGE('',*,*,#8185,.F.);
#11283=ORIENTED_EDGE('',*,*,#8186,.F.);
#11284=ORIENTED_EDGE('',*,*,#8048,.F.);
#11285=ORIENTED_EDGE('',*,*,#8186,.T.);
#11286=ORIENTED_EDGE('',*,*,#8187,.F.);
#11287=ORIENTED_EDGE('',*,*,#8188,.F.);
#11288=ORIENTED_EDGE('',*,*,#8049,.F.);
#11289=ORIENTED_EDGE('',*,*,#8188,.T.);
#11290=ORIENTED_EDGE('',*,*,#8189,.F.);
#11291=ORIENTED_EDGE('',*,*,#8190,.F.);
#11292=ORIENTED_EDGE('',*,*,#8050,.F.);
#11293=ORIENTED_EDGE('',*,*,#8190,.T.);
#11294=ORIENTED_EDGE('',*,*,#8191,.F.);
#11295=ORIENTED_EDGE('',*,*,#8192,.T.);
#11296=ORIENTED_EDGE('',*,*,#8051,.F.);
#11297=ORIENTED_EDGE('',*,*,#8192,.F.);
#11298=ORIENTED_EDGE('',*,*,#8193,.F.);
#11299=ORIENTED_EDGE('',*,*,#8194,.F.);
#11300=ORIENTED_EDGE('',*,*,#8052,.F.);
#11301=ORIENTED_EDGE('',*,*,#8194,.T.);
#11302=ORIENTED_EDGE('',*,*,#8195,.F.);
#11303=ORIENTED_EDGE('',*,*,#8196,.F.);
#11304=ORIENTED_EDGE('',*,*,#8053,.F.);
#11305=ORIENTED_EDGE('',*,*,#8196,.T.);
#11306=ORIENTED_EDGE('',*,*,#8197,.F.);
#11307=ORIENTED_EDGE('',*,*,#8198,.F.);
#11308=ORIENTED_EDGE('',*,*,#8054,.F.);
#11309=ORIENTED_EDGE('',*,*,#8198,.T.);
#11310=ORIENTED_EDGE('',*,*,#8199,.F.);
#11311=ORIENTED_EDGE('',*,*,#8200,.T.);
#11312=ORIENTED_EDGE('',*,*,#8055,.F.);
#11313=ORIENTED_EDGE('',*,*,#8200,.F.);
#11314=ORIENTED_EDGE('',*,*,#8201,.F.);
#11315=ORIENTED_EDGE('',*,*,#8202,.F.);
#11316=ORIENTED_EDGE('',*,*,#8056,.F.);
#11317=ORIENTED_EDGE('',*,*,#8202,.T.);
#11318=ORIENTED_EDGE('',*,*,#8203,.F.);
#11319=ORIENTED_EDGE('',*,*,#8204,.F.);
#11320=ORIENTED_EDGE('',*,*,#8057,.F.);
#11321=ORIENTED_EDGE('',*,*,#8204,.T.);
#11322=ORIENTED_EDGE('',*,*,#8205,.F.);
#11323=ORIENTED_EDGE('',*,*,#8206,.F.);
#11324=ORIENTED_EDGE('',*,*,#8058,.F.);
#11325=ORIENTED_EDGE('',*,*,#8206,.T.);
#11326=ORIENTED_EDGE('',*,*,#8207,.F.);
#11327=ORIENTED_EDGE('',*,*,#8208,.T.);
#11328=ORIENTED_EDGE('',*,*,#8059,.F.);
#11329=ORIENTED_EDGE('',*,*,#8208,.F.);
#11330=ORIENTED_EDGE('',*,*,#8209,.F.);
#11331=ORIENTED_EDGE('',*,*,#8210,.F.);
#11332=ORIENTED_EDGE('',*,*,#8060,.F.);
#11333=ORIENTED_EDGE('',*,*,#8210,.T.);
#11334=ORIENTED_EDGE('',*,*,#8211,.F.);
#11335=ORIENTED_EDGE('',*,*,#8212,.F.);
#11336=ORIENTED_EDGE('',*,*,#8061,.F.);
#11337=ORIENTED_EDGE('',*,*,#8212,.T.);
#11338=ORIENTED_EDGE('',*,*,#8213,.F.);
#11339=ORIENTED_EDGE('',*,*,#8214,.F.);
#11340=ORIENTED_EDGE('',*,*,#8062,.F.);
#11341=ORIENTED_EDGE('',*,*,#8214,.T.);
#11342=ORIENTED_EDGE('',*,*,#8215,.F.);
#11343=ORIENTED_EDGE('',*,*,#8216,.T.);
#11344=ORIENTED_EDGE('',*,*,#8063,.F.);
#11345=ORIENTED_EDGE('',*,*,#8216,.F.);
#11346=ORIENTED_EDGE('',*,*,#8217,.F.);
#11347=ORIENTED_EDGE('',*,*,#8218,.F.);
#11348=ORIENTED_EDGE('',*,*,#8064,.F.);
#11349=ORIENTED_EDGE('',*,*,#8218,.T.);
#11350=ORIENTED_EDGE('',*,*,#8219,.F.);
#11351=ORIENTED_EDGE('',*,*,#8220,.F.);
#11352=ORIENTED_EDGE('',*,*,#8065,.F.);
#11353=ORIENTED_EDGE('',*,*,#8220,.T.);
#11354=ORIENTED_EDGE('',*,*,#8221,.F.);
#11355=ORIENTED_EDGE('',*,*,#8222,.F.);
#11356=ORIENTED_EDGE('',*,*,#8066,.F.);
#11357=ORIENTED_EDGE('',*,*,#8222,.T.);
#11358=ORIENTED_EDGE('',*,*,#8223,.F.);
#11359=ORIENTED_EDGE('',*,*,#8224,.T.);
#11360=ORIENTED_EDGE('',*,*,#8067,.F.);
#11361=ORIENTED_EDGE('',*,*,#8224,.F.);
#11362=ORIENTED_EDGE('',*,*,#8225,.F.);
#11363=ORIENTED_EDGE('',*,*,#8226,.F.);
#11364=ORIENTED_EDGE('',*,*,#8068,.F.);
#11365=ORIENTED_EDGE('',*,*,#8226,.T.);
#11366=ORIENTED_EDGE('',*,*,#8227,.F.);
#11367=ORIENTED_EDGE('',*,*,#8228,.F.);
#11368=ORIENTED_EDGE('',*,*,#8069,.F.);
#11369=ORIENTED_EDGE('',*,*,#8228,.T.);
#11370=ORIENTED_EDGE('',*,*,#8229,.F.);
#11371=ORIENTED_EDGE('',*,*,#8230,.F.);
#11372=ORIENTED_EDGE('',*,*,#8070,.F.);
#11373=ORIENTED_EDGE('',*,*,#8230,.T.);
#11374=ORIENTED_EDGE('',*,*,#8231,.F.);
#11375=ORIENTED_EDGE('',*,*,#8232,.T.);
#11376=ORIENTED_EDGE('',*,*,#8071,.F.);
#11377=ORIENTED_EDGE('',*,*,#8232,.F.);
#11378=ORIENTED_EDGE('',*,*,#8233,.F.);
#11379=ORIENTED_EDGE('',*,*,#8234,.F.);
#11380=ORIENTED_EDGE('',*,*,#8072,.F.);
#11381=ORIENTED_EDGE('',*,*,#8234,.T.);
#11382=ORIENTED_EDGE('',*,*,#8235,.F.);
#11383=ORIENTED_EDGE('',*,*,#8236,.F.);
#11384=ORIENTED_EDGE('',*,*,#8073,.F.);
#11385=ORIENTED_EDGE('',*,*,#8236,.T.);
#11386=ORIENTED_EDGE('',*,*,#8237,.F.);
#11387=ORIENTED_EDGE('',*,*,#8238,.F.);
#11388=ORIENTED_EDGE('',*,*,#8074,.F.);
#11389=ORIENTED_EDGE('',*,*,#8238,.T.);
#11390=ORIENTED_EDGE('',*,*,#8239,.F.);
#11391=ORIENTED_EDGE('',*,*,#8240,.T.);
#11392=ORIENTED_EDGE('',*,*,#8075,.F.);
#11393=ORIENTED_EDGE('',*,*,#8240,.F.);
#11394=ORIENTED_EDGE('',*,*,#8241,.F.);
#11395=ORIENTED_EDGE('',*,*,#8242,.F.);
#11396=ORIENTED_EDGE('',*,*,#8076,.F.);
#11397=ORIENTED_EDGE('',*,*,#8242,.T.);
#11398=ORIENTED_EDGE('',*,*,#8243,.F.);
#11399=ORIENTED_EDGE('',*,*,#8244,.F.);
#11400=ORIENTED_EDGE('',*,*,#8077,.F.);
#11401=ORIENTED_EDGE('',*,*,#8244,.T.);
#11402=ORIENTED_EDGE('',*,*,#8245,.F.);
#11403=ORIENTED_EDGE('',*,*,#8246,.F.);
#11404=ORIENTED_EDGE('',*,*,#8078,.F.);
#11405=ORIENTED_EDGE('',*,*,#8247,.T.);
#11406=ORIENTED_EDGE('',*,*,#8245,.T.);
#11407=ORIENTED_EDGE('',*,*,#8243,.T.);
#11408=ORIENTED_EDGE('',*,*,#8241,.T.);
#11409=ORIENTED_EDGE('',*,*,#8239,.T.);
#11410=ORIENTED_EDGE('',*,*,#8237,.T.);
#11411=ORIENTED_EDGE('',*,*,#8235,.T.);
#11412=ORIENTED_EDGE('',*,*,#8233,.T.);
#11413=ORIENTED_EDGE('',*,*,#8231,.T.);
#11414=ORIENTED_EDGE('',*,*,#8229,.T.);
#11415=ORIENTED_EDGE('',*,*,#8227,.T.);
#11416=ORIENTED_EDGE('',*,*,#8225,.T.);
#11417=ORIENTED_EDGE('',*,*,#8223,.T.);
#11418=ORIENTED_EDGE('',*,*,#8221,.T.);
#11419=ORIENTED_EDGE('',*,*,#8219,.T.);
#11420=ORIENTED_EDGE('',*,*,#8217,.T.);
#11421=ORIENTED_EDGE('',*,*,#8215,.T.);
#11422=ORIENTED_EDGE('',*,*,#8213,.T.);
#11423=ORIENTED_EDGE('',*,*,#8211,.T.);
#11424=ORIENTED_EDGE('',*,*,#8209,.T.);
#11425=ORIENTED_EDGE('',*,*,#8207,.T.);
#11426=ORIENTED_EDGE('',*,*,#8205,.T.);
#11427=ORIENTED_EDGE('',*,*,#8203,.T.);
#11428=ORIENTED_EDGE('',*,*,#8201,.T.);
#11429=ORIENTED_EDGE('',*,*,#8199,.T.);
#11430=ORIENTED_EDGE('',*,*,#8197,.T.);
#11431=ORIENTED_EDGE('',*,*,#8195,.T.);
#11432=ORIENTED_EDGE('',*,*,#8193,.T.);
#11433=ORIENTED_EDGE('',*,*,#8191,.T.);
#11434=ORIENTED_EDGE('',*,*,#8189,.T.);
#11435=ORIENTED_EDGE('',*,*,#8187,.T.);
#11436=ORIENTED_EDGE('',*,*,#8185,.T.);
#11437=ORIENTED_EDGE('',*,*,#8183,.T.);
#11438=ORIENTED_EDGE('',*,*,#8181,.T.);
#11439=ORIENTED_EDGE('',*,*,#8179,.T.);
#11440=ORIENTED_EDGE('',*,*,#8177,.T.);
#11441=ORIENTED_EDGE('',*,*,#8175,.T.);
#11442=ORIENTED_EDGE('',*,*,#8173,.T.);
#11443=ORIENTED_EDGE('',*,*,#8171,.T.);
#11444=ORIENTED_EDGE('',*,*,#8169,.T.);
#11445=ORIENTED_EDGE('',*,*,#8167,.T.);
#11446=ORIENTED_EDGE('',*,*,#8165,.T.);
#11447=ORIENTED_EDGE('',*,*,#8163,.T.);
#11448=ORIENTED_EDGE('',*,*,#8161,.T.);
#11449=ORIENTED_EDGE('',*,*,#8159,.T.);
#11450=ORIENTED_EDGE('',*,*,#8157,.T.);
#11451=ORIENTED_EDGE('',*,*,#8155,.T.);
#11452=ORIENTED_EDGE('',*,*,#8153,.T.);
#11453=ORIENTED_EDGE('',*,*,#8151,.T.);
#11454=ORIENTED_EDGE('',*,*,#8149,.T.);
#11455=ORIENTED_EDGE('',*,*,#8147,.T.);
#11456=ORIENTED_EDGE('',*,*,#8145,.T.);
#11457=ORIENTED_EDGE('',*,*,#8143,.T.);
#11458=ORIENTED_EDGE('',*,*,#8141,.T.);
#11459=ORIENTED_EDGE('',*,*,#8139,.T.);
#11460=ORIENTED_EDGE('',*,*,#8137,.T.);
#11461=ORIENTED_EDGE('',*,*,#8135,.T.);
#11462=ORIENTED_EDGE('',*,*,#8133,.T.);
#11463=ORIENTED_EDGE('',*,*,#8131,.T.);
#11464=ORIENTED_EDGE('',*,*,#8129,.T.);
#11465=ORIENTED_EDGE('',*,*,#8127,.T.);
#11466=ORIENTED_EDGE('',*,*,#8125,.T.);
#11467=ORIENTED_EDGE('',*,*,#8123,.T.);
#11468=ORIENTED_EDGE('',*,*,#8121,.T.);
#11469=ORIENTED_EDGE('',*,*,#8119,.T.);
#11470=ORIENTED_EDGE('',*,*,#8117,.T.);
#11471=ORIENTED_EDGE('',*,*,#8115,.T.);
#11472=ORIENTED_EDGE('',*,*,#8113,.T.);
#11473=ORIENTED_EDGE('',*,*,#8111,.T.);
#11474=ORIENTED_EDGE('',*,*,#8109,.T.);
#11475=ORIENTED_EDGE('',*,*,#8107,.T.);
#11476=ORIENTED_EDGE('',*,*,#8105,.T.);
#11477=ORIENTED_EDGE('',*,*,#8103,.T.);
#11478=ORIENTED_EDGE('',*,*,#8101,.T.);
#11479=ORIENTED_EDGE('',*,*,#8099,.T.);
#11480=ORIENTED_EDGE('',*,*,#8097,.T.);
#11481=ORIENTED_EDGE('',*,*,#8095,.T.);
#11482=ORIENTED_EDGE('',*,*,#8093,.T.);
#11483=ORIENTED_EDGE('',*,*,#8091,.T.);
#11484=ORIENTED_EDGE('',*,*,#8089,.T.);
#11485=ORIENTED_EDGE('',*,*,#8087,.T.);
#11486=ORIENTED_EDGE('',*,*,#8088,.T.);
#11487=ORIENTED_EDGE('',*,*,#8079,.F.);
#11488=ORIENTED_EDGE('',*,*,#8246,.T.);
#11489=ORIENTED_EDGE('',*,*,#8247,.F.);
#11490=ORIENTED_EDGE('',*,*,#8248,.F.);
#11491=ORIENTED_EDGE('',*,*,#8249,.T.);
#11492=ORIENTED_EDGE('',*,*,#8250,.T.);
#11493=ORIENTED_EDGE('',*,*,#8249,.F.);
#11494=ORIENTED_EDGE('',*,*,#8251,.F.);
#11495=ORIENTED_EDGE('',*,*,#8252,.T.);
#11496=ORIENTED_EDGE('',*,*,#8253,.T.);
#11497=ORIENTED_EDGE('',*,*,#8252,.F.);
#11498=ORIENTED_EDGE('',*,*,#8251,.T.);
#11499=ORIENTED_EDGE('',*,*,#8248,.T.);
#11500=ORIENTED_EDGE('',*,*,#8253,.F.);
#11501=ORIENTED_EDGE('',*,*,#8250,.F.);
#11502=ORIENTED_EDGE('',*,*,#8254,.F.);
#11503=ORIENTED_EDGE('',*,*,#8255,.F.);
#11504=ORIENTED_EDGE('',*,*,#8256,.T.);
#11505=ORIENTED_EDGE('',*,*,#8254,.T.);
#11506=ORIENTED_EDGE('',*,*,#8256,.F.);
#11507=ORIENTED_EDGE('',*,*,#8257,.F.);
#11508=ORIENTED_EDGE('',*,*,#8258,.T.);
#11509=ORIENTED_EDGE('',*,*,#8255,.T.);
#11510=ORIENTED_EDGE('',*,*,#8258,.F.);
#11511=ORIENTED_EDGE('',*,*,#8259,.F.);
#11512=ORIENTED_EDGE('',*,*,#8260,.T.);
#11513=ORIENTED_EDGE('',*,*,#8257,.T.);
#11514=ORIENTED_EDGE('',*,*,#8260,.F.);
#11515=ORIENTED_EDGE('',*,*,#8259,.T.);
#11516=ORIENTED_EDGE('',*,*,#8261,.F.);
#11517=ORIENTED_EDGE('',*,*,#8262,.F.);
#11518=ORIENTED_EDGE('',*,*,#8263,.T.);
#11519=ORIENTED_EDGE('',*,*,#8261,.T.);
#11520=ORIENTED_EDGE('',*,*,#8263,.F.);
#11521=ORIENTED_EDGE('',*,*,#8264,.F.);
#11522=ORIENTED_EDGE('',*,*,#8265,.T.);
#11523=ORIENTED_EDGE('',*,*,#8262,.T.);
#11524=ORIENTED_EDGE('',*,*,#8265,.F.);
#11525=ORIENTED_EDGE('',*,*,#8266,.F.);
#11526=ORIENTED_EDGE('',*,*,#8267,.T.);
#11527=ORIENTED_EDGE('',*,*,#8264,.T.);
#11528=ORIENTED_EDGE('',*,*,#8267,.F.);
#11529=ORIENTED_EDGE('',*,*,#8266,.T.);
#11530=ORIENTED_EDGE('',*,*,#8268,.T.);
#11531=ORIENTED_EDGE('',*,*,#8269,.T.);
#11532=ORIENTED_EDGE('',*,*,#8270,.T.);
#11533=ORIENTED_EDGE('',*,*,#8271,.F.);
#11534=ORIENTED_EDGE('',*,*,#8272,.T.);
#11535=ORIENTED_EDGE('',*,*,#8273,.T.);
#11536=ORIENTED_EDGE('',*,*,#8274,.T.);
#11537=ORIENTED_EDGE('',*,*,#8269,.F.);
#11538=ORIENTED_EDGE('',*,*,#8275,.T.);
#11539=ORIENTED_EDGE('',*,*,#8276,.T.);
#11540=ORIENTED_EDGE('',*,*,#8277,.T.);
#11541=ORIENTED_EDGE('',*,*,#8273,.F.);
#11542=ORIENTED_EDGE('',*,*,#8278,.T.);
#11543=ORIENTED_EDGE('',*,*,#8279,.T.);
#11544=ORIENTED_EDGE('',*,*,#8280,.T.);
#11545=ORIENTED_EDGE('',*,*,#8276,.F.);
#11546=ORIENTED_EDGE('',*,*,#8281,.T.);
#11547=ORIENTED_EDGE('',*,*,#8282,.T.);
#11548=ORIENTED_EDGE('',*,*,#8283,.T.);
#11549=ORIENTED_EDGE('',*,*,#8279,.F.);
#11550=ORIENTED_EDGE('',*,*,#8284,.T.);
#11551=ORIENTED_EDGE('',*,*,#8271,.T.);
#11552=ORIENTED_EDGE('',*,*,#8285,.T.);
#11553=ORIENTED_EDGE('',*,*,#8282,.F.);
#11554=ORIENTED_EDGE('',*,*,#8284,.F.);
#11555=ORIENTED_EDGE('',*,*,#8281,.F.);
#11556=ORIENTED_EDGE('',*,*,#8278,.F.);
#11557=ORIENTED_EDGE('',*,*,#8275,.F.);
#11558=ORIENTED_EDGE('',*,*,#8272,.F.);
#11559=ORIENTED_EDGE('',*,*,#8268,.F.);
#11560=ORIENTED_EDGE('',*,*,#8285,.F.);
#11561=ORIENTED_EDGE('',*,*,#8270,.F.);
#11562=ORIENTED_EDGE('',*,*,#8274,.F.);
#11563=ORIENTED_EDGE('',*,*,#8277,.F.);
#11564=ORIENTED_EDGE('',*,*,#8280,.F.);
#11565=ORIENTED_EDGE('',*,*,#8283,.F.);
#11566=ORIENTED_EDGE('',*,*,#8286,.F.);
#11567=ORIENTED_EDGE('',*,*,#8287,.F.);
#11568=ORIENTED_EDGE('',*,*,#8288,.T.);
#11569=ORIENTED_EDGE('',*,*,#8286,.T.);
#11570=ORIENTED_EDGE('',*,*,#8288,.F.);
#11571=ORIENTED_EDGE('',*,*,#8289,.F.);
#11572=ORIENTED_EDGE('',*,*,#8290,.T.);
#11573=ORIENTED_EDGE('',*,*,#8287,.T.);
#11574=ORIENTED_EDGE('',*,*,#8290,.F.);
#11575=ORIENTED_EDGE('',*,*,#8291,.F.);
#11576=ORIENTED_EDGE('',*,*,#8292,.T.);
#11577=ORIENTED_EDGE('',*,*,#8289,.T.);
#11578=ORIENTED_EDGE('',*,*,#8292,.F.);
#11579=ORIENTED_EDGE('',*,*,#8291,.T.);
#11580=ORIENTED_EDGE('',*,*,#8293,.F.);
#11581=ORIENTED_EDGE('',*,*,#8294,.F.);
#11582=ORIENTED_EDGE('',*,*,#8295,.T.);
#11583=ORIENTED_EDGE('',*,*,#8293,.T.);
#11584=ORIENTED_EDGE('',*,*,#8295,.F.);
#11585=ORIENTED_EDGE('',*,*,#8296,.F.);
#11586=ORIENTED_EDGE('',*,*,#8297,.T.);
#11587=ORIENTED_EDGE('',*,*,#8294,.T.);
#11588=ORIENTED_EDGE('',*,*,#8297,.F.);
#11589=ORIENTED_EDGE('',*,*,#8298,.F.);
#11590=ORIENTED_EDGE('',*,*,#8299,.T.);
#11591=ORIENTED_EDGE('',*,*,#8296,.T.);
#11592=ORIENTED_EDGE('',*,*,#8299,.F.);
#11593=ORIENTED_EDGE('',*,*,#8298,.T.);
#11594=ORIENTED_EDGE('',*,*,#8300,.T.);
#11595=ORIENTED_EDGE('',*,*,#8301,.T.);
#11596=ORIENTED_EDGE('',*,*,#8302,.T.);
#11597=ORIENTED_EDGE('',*,*,#8303,.F.);
#11598=ORIENTED_EDGE('',*,*,#8304,.T.);
#11599=ORIENTED_EDGE('',*,*,#8305,.T.);
#11600=ORIENTED_EDGE('',*,*,#8306,.T.);
#11601=ORIENTED_EDGE('',*,*,#8301,.F.);
#11602=ORIENTED_EDGE('',*,*,#8307,.T.);
#11603=ORIENTED_EDGE('',*,*,#8308,.T.);
#11604=ORIENTED_EDGE('',*,*,#8309,.T.);
#11605=ORIENTED_EDGE('',*,*,#8305,.F.);
#11606=ORIENTED_EDGE('',*,*,#8310,.T.);
#11607=ORIENTED_EDGE('',*,*,#8311,.T.);
#11608=ORIENTED_EDGE('',*,*,#8312,.T.);
#11609=ORIENTED_EDGE('',*,*,#8308,.F.);
#11610=ORIENTED_EDGE('',*,*,#8313,.T.);
#11611=ORIENTED_EDGE('',*,*,#8314,.T.);
#11612=ORIENTED_EDGE('',*,*,#8315,.T.);
#11613=ORIENTED_EDGE('',*,*,#8311,.F.);
#11614=ORIENTED_EDGE('',*,*,#8316,.T.);
#11615=ORIENTED_EDGE('',*,*,#8303,.T.);
#11616=ORIENTED_EDGE('',*,*,#8317,.T.);
#11617=ORIENTED_EDGE('',*,*,#8314,.F.);
#11618=ORIENTED_EDGE('',*,*,#8316,.F.);
#11619=ORIENTED_EDGE('',*,*,#8313,.F.);
#11620=ORIENTED_EDGE('',*,*,#8310,.F.);
#11621=ORIENTED_EDGE('',*,*,#8307,.F.);
#11622=ORIENTED_EDGE('',*,*,#8304,.F.);
#11623=ORIENTED_EDGE('',*,*,#8300,.F.);
#11624=ORIENTED_EDGE('',*,*,#8317,.F.);
#11625=ORIENTED_EDGE('',*,*,#8302,.F.);
#11626=ORIENTED_EDGE('',*,*,#8306,.F.);
#11627=ORIENTED_EDGE('',*,*,#8309,.F.);
#11628=ORIENTED_EDGE('',*,*,#8312,.F.);
#11629=ORIENTED_EDGE('',*,*,#8315,.F.);
#11630=ORIENTED_EDGE('',*,*,#8318,.F.);
#11631=ORIENTED_EDGE('',*,*,#8319,.T.);
#11632=ORIENTED_EDGE('',*,*,#8320,.T.);
#11633=ORIENTED_EDGE('',*,*,#8319,.F.);
#11634=ORIENTED_EDGE('',*,*,#8321,.F.);
#11635=ORIENTED_EDGE('',*,*,#8322,.T.);
#11636=ORIENTED_EDGE('',*,*,#8323,.T.);
#11637=ORIENTED_EDGE('',*,*,#8322,.F.);
#11638=ORIENTED_EDGE('',*,*,#8321,.T.);
#11639=ORIENTED_EDGE('',*,*,#8318,.T.);
#11640=ORIENTED_EDGE('',*,*,#8323,.F.);
#11641=ORIENTED_EDGE('',*,*,#8320,.F.);
#11642=CYLINDRICAL_SURFACE('',#13002,0.165);
#11643=CYLINDRICAL_SURFACE('',#13005,0.165);
#11644=CYLINDRICAL_SURFACE('',#13008,0.165);
#11645=CYLINDRICAL_SURFACE('',#13011,0.165);
#11646=CYLINDRICAL_SURFACE('',#13014,0.165);
#11647=CYLINDRICAL_SURFACE('',#13017,0.165);
#11648=CYLINDRICAL_SURFACE('',#13020,0.21);
#11649=CYLINDRICAL_SURFACE('',#13023,0.21);
#11650=CYLINDRICAL_SURFACE('',#13026,0.21);
#11651=CYLINDRICAL_SURFACE('',#13029,0.21);
#11652=CYLINDRICAL_SURFACE('',#13053,0.165);
#11653=CYLINDRICAL_SURFACE('',#13057,0.165);
#11654=CYLINDRICAL_SURFACE('',#13067,1.4);
#11655=CYLINDRICAL_SURFACE('',#13069,2.);
#11656=CYLINDRICAL_SURFACE('',#13071,2.);
#11657=CYLINDRICAL_SURFACE('',#13076,0.165);
#11658=CYLINDRICAL_SURFACE('',#13080,0.165);
#11659=CYLINDRICAL_SURFACE('',#13090,1.4);
#11660=CYLINDRICAL_SURFACE('',#13092,2.);
#11661=CYLINDRICAL_SURFACE('',#13094,2.);
#11662=CYLINDRICAL_SURFACE('',#13099,0.275);
#11663=CYLINDRICAL_SURFACE('',#13102,0.275);
#11664=CYLINDRICAL_SURFACE('',#13105,0.275);
#11665=CYLINDRICAL_SURFACE('',#13108,0.275);
#11666=CYLINDRICAL_SURFACE('',#13130,1.005);
#11667=CYLINDRICAL_SURFACE('',#13132,1.4);
#11668=CYLINDRICAL_SURFACE('',#13136,1.6);
#11669=CYLINDRICAL_SURFACE('',#13140,0.225);
#11670=CYLINDRICAL_SURFACE('',#13143,0.225);
#11671=CYLINDRICAL_SURFACE('',#13154,1.01);
#11672=CYLINDRICAL_SURFACE('',#13168,1.005);
#11673=CYLINDRICAL_SURFACE('',#13170,1.4);
#11674=CYLINDRICAL_SURFACE('',#13174,1.6);
#11675=CYLINDRICAL_SURFACE('',#13178,0.225);
#11676=CYLINDRICAL_SURFACE('',#13181,0.225);
#11677=CYLINDRICAL_SURFACE('',#13192,1.01);
#11678=CYLINDRICAL_SURFACE('',#13199,0.4);
#11679=CYLINDRICAL_SURFACE('',#13204,0.4);
#11680=CYLINDRICAL_SURFACE('',#13209,0.225);
#11681=CYLINDRICAL_SURFACE('',#13211,0.225);
#11682=CYLINDRICAL_SURFACE('',#13213,2.5);
#11683=CYLINDRICAL_SURFACE('',#13219,2.52);
#11684=CYLINDRICAL_SURFACE('',#13226,0.165);
#11685=CYLINDRICAL_SURFACE('',#13229,0.165);
#11686=CYLINDRICAL_SURFACE('',#13232,0.165);
#11687=CYLINDRICAL_SURFACE('',#13235,0.165);
#11688=CYLINDRICAL_SURFACE('',#13238,0.225);
#11689=CYLINDRICAL_SURFACE('',#13240,0.225);
#11690=CYLINDRICAL_SURFACE('',#13242,1.6);
#11691=CYLINDRICAL_SURFACE('',#13254,1.41);
#11692=CYLINDRICAL_SURFACE('',#13257,0.225);
#11693=CYLINDRICAL_SURFACE('',#13260,0.225);
#11694=CYLINDRICAL_SURFACE('',#13263,0.225);
#11695=CYLINDRICAL_SURFACE('',#13266,0.225);
#11696=CYLINDRICAL_SURFACE('',#13269,1.59);
#11697=CYLINDRICAL_SURFACE('',#13273,2.4);
#11698=CYLINDRICAL_SURFACE('',#13279,1.41);
#11699=CYLINDRICAL_SURFACE('',#13282,0.225);
#11700=CYLINDRICAL_SURFACE('',#13285,0.225);
#11701=CYLINDRICAL_SURFACE('',#13288,0.225);
#11702=CYLINDRICAL_SURFACE('',#13291,0.225);
#11703=CYLINDRICAL_SURFACE('',#13294,1.59);
#11704=CYLINDRICAL_SURFACE('',#13298,2.4);
#11705=CYLINDRICAL_SURFACE('',#13304,2.52);
#11706=CYLINDRICAL_SURFACE('',#13316,0.165);
#11707=CYLINDRICAL_SURFACE('',#13318,0.165);
#11708=CYLINDRICAL_SURFACE('',#13320,0.165);
#11709=CYLINDRICAL_SURFACE('',#13322,0.165);
#11710=CYLINDRICAL_SURFACE('',#13324,0.225);
#11711=CYLINDRICAL_SURFACE('',#13326,0.225);
#11712=CYLINDRICAL_SURFACE('',#13328,1.6);
#11713=CYLINDRICAL_SURFACE('',#13339,1.41);
#11714=CYLINDRICAL_SURFACE('',#13342,0.225);
#11715=CYLINDRICAL_SURFACE('',#13345,0.225);
#11716=CYLINDRICAL_SURFACE('',#13348,0.225);
#11717=CYLINDRICAL_SURFACE('',#13351,0.225);
#11718=CYLINDRICAL_SURFACE('',#13354,1.59);
#11719=CYLINDRICAL_SURFACE('',#13358,2.4);
#11720=CYLINDRICAL_SURFACE('',#13364,1.41);
#11721=CYLINDRICAL_SURFACE('',#13367,0.225);
#11722=CYLINDRICAL_SURFACE('',#13370,0.225);
#11723=CYLINDRICAL_SURFACE('',#13373,0.225);
#11724=CYLINDRICAL_SURFACE('',#13376,0.225);
#11725=CYLINDRICAL_SURFACE('',#13379,1.59);
#11726=CYLINDRICAL_SURFACE('',#13383,2.4);
#11727=CYLINDRICAL_SURFACE('',#13393,0.425);
#11728=CYLINDRICAL_SURFACE('',#13401,0.24505);
#11729=CYLINDRICAL_SURFACE('',#13422,1.070235);
#11730=CYLINDRICAL_SURFACE('',#13424,0.6);
#11731=CYLINDRICAL_SURFACE('',#13430,1.070235);
#11732=CYLINDRICAL_SURFACE('',#13442,1.129765);
#11733=CYLINDRICAL_SURFACE('',#13449,1.6);
#11734=CYLINDRICAL_SURFACE('',#13454,1.129765);
#11735=CYLINDRICAL_SURFACE('',#13474,1.123812);
#11736=CYLINDRICAL_SURFACE('',#13510,1.076188);
#11737=CYLINDRICAL_SURFACE('',#13524,1.119765);
#11738=CYLINDRICAL_SURFACE('',#13528,1.085235);
#11739=CYLINDRICAL_SURFACE('',#13532,1.119765);
#11740=CYLINDRICAL_SURFACE('',#13536,1.085235);
#11741=CYLINDRICAL_SURFACE('',#13557,0.35);
#11742=CYLINDRICAL_SURFACE('',#13565,0.1954);
#11743=CYLINDRICAL_SURFACE('',#13568,0.425);
#11744=CYLINDRICAL_SURFACE('',#13743,1.);
#11745=CYLINDRICAL_SURFACE('',#13749,0.5);
#11746=CYLINDRICAL_SURFACE('',#13753,1.2);
#11747=CYLINDRICAL_SURFACE('',#13759,0.164999999999999);
#11748=CYLINDRICAL_SURFACE('',#13767,1.7);
#11749=CYLINDRICAL_SURFACE('',#13769,1.005);
#11750=CYLINDRICAL_SURFACE('',#13784,0.1954);
#11751=CYLINDRICAL_SURFACE('',#13795,0.165);
#11752=CYLINDRICAL_SURFACE('',#13799,0.165);
#11753=CYLINDRICAL_SURFACE('',#13817,0.6);
#11754=CYLINDRICAL_SURFACE('',#13823,0.605);
#11755=CYLINDRICAL_SURFACE('',#13826,0.8);
#11756=CYLINDRICAL_SURFACE('',#13832,0.605);
#11757=CYLINDRICAL_SURFACE('',#13835,0.8);
#11758=CYLINDRICAL_SURFACE('',#13841,0.605);
#11759=CYLINDRICAL_SURFACE('',#13844,0.8);
#11760=CYLINDRICAL_SURFACE('',#13850,0.605);
#11761=CYLINDRICAL_SURFACE('',#13853,0.8);
#11762=CYLINDRICAL_SURFACE('',#13873,0.25);
#11763=CYLINDRICAL_SURFACE('',#13882,0.6);
#11764=CYLINDRICAL_SURFACE('',#13884,0.9);
#11765=CYLINDRICAL_SURFACE('',#13893,1.3);
#11766=CYLINDRICAL_SURFACE('',#13897,0.33);
#11767=CYLINDRICAL_SURFACE('',#13900,0.4);
#11768=CYLINDRICAL_SURFACE('',#13906,0.225);
#11769=CYLINDRICAL_SURFACE('',#13909,1.);
#11770=CYLINDRICAL_SURFACE('',#13915,0.225);
#11771=CYLINDRICAL_SURFACE('',#13918,1.);
#11772=CYLINDRICAL_SURFACE('',#13949,0.6);
#11773=CYLINDRICAL_SURFACE('',#13951,1.4);
#11774=CYLINDRICAL_SURFACE('',#13956,1.75);
#11775=CYLINDRICAL_SURFACE('',#13959,1.75);
#11776=CYLINDRICAL_SURFACE('',#13962,1.75);
#11777=CYLINDRICAL_SURFACE('',#13965,1.75);
#11778=CYLINDRICAL_SURFACE('',#13968,1.75);
#11779=CYLINDRICAL_SURFACE('',#13971,1.75);
#11780=CYLINDRICAL_SURFACE('',#13974,1.75);
#11781=CYLINDRICAL_SURFACE('',#13977,1.75);
#11782=CYLINDRICAL_SURFACE('',#13980,1.75);
#11783=CYLINDRICAL_SURFACE('',#13983,1.75);
#11784=CYLINDRICAL_SURFACE('',#13986,1.75);
#11785=CYLINDRICAL_SURFACE('',#13989,1.75);
#11786=CYLINDRICAL_SURFACE('',#13992,1.75);
#11787=CYLINDRICAL_SURFACE('',#13995,1.75);
#11788=CYLINDRICAL_SURFACE('',#13998,1.75);
#11789=CYLINDRICAL_SURFACE('',#14001,1.75);
#11790=CYLINDRICAL_SURFACE('',#14004,1.75);
#11791=CYLINDRICAL_SURFACE('',#14007,1.75);
#11792=CYLINDRICAL_SURFACE('',#14010,1.75);
#11793=CYLINDRICAL_SURFACE('',#14015,1.75);
#11794=CYLINDRICAL_SURFACE('',#14017,0.32);
#11795=CYLINDRICAL_SURFACE('',#14020,0.6);
#11796=CYLINDRICAL_SURFACE('',#14030,0.5);
#11797=CYLINDRICAL_SURFACE('',#14038,0.2942);
#11798=CYLINDRICAL_SURFACE('',#14056,0.35);
#11799=CYLINDRICAL_SURFACE('',#14064,0.1954);
#11800=CYLINDRICAL_SURFACE('',#14142,0.405);
#11801=CYLINDRICAL_SURFACE('',#14145,0.9);
#11802=ADVANCED_FACE('',(#1293),#11642,.F.);
#11803=ADVANCED_FACE('',(#1294),#11643,.F.);
#11804=ADVANCED_FACE('',(#1295),#11644,.F.);
#11805=ADVANCED_FACE('',(#1296),#11645,.F.);
#11806=ADVANCED_FACE('',(#1297),#11646,.F.);
#11807=ADVANCED_FACE('',(#1298),#11647,.F.);
#11808=ADVANCED_FACE('',(#1299),#11648,.F.);
#11809=ADVANCED_FACE('',(#1300),#11649,.F.);
#11810=ADVANCED_FACE('',(#1301),#11650,.F.);
#11811=ADVANCED_FACE('',(#1302),#11651,.F.);
#11812=ADVANCED_FACE('',(#1303),#849,.T.);
#11813=ADVANCED_FACE('',(#1304),#850,.T.);
#11814=ADVANCED_FACE('',(#1305),#851,.T.);
#11815=ADVANCED_FACE('',(#1306),#852,.T.);
#11816=ADVANCED_FACE('',(#1307,#680,#681,#682,#683,#684,#685,#686,#687,
#688,#689),#853,.T.);
#11817=ADVANCED_FACE('',(#1308,#690,#691,#692,#693,#694,#695,#696,#697,
#698,#699),#854,.F.);
#11818=ADVANCED_FACE('',(#1309),#855,.T.);
#11819=ADVANCED_FACE('',(#1310),#856,.T.);
#11820=ADVANCED_FACE('',(#1311),#857,.T.);
#11821=ADVANCED_FACE('',(#1312),#858,.T.);
#11822=ADVANCED_FACE('',(#1313),#859,.T.);
#11823=ADVANCED_FACE('',(#1314),#860,.F.);
#11824=ADVANCED_FACE('',(#1315),#861,.T.);
#11825=ADVANCED_FACE('',(#1316),#862,.T.);
#11826=ADVANCED_FACE('',(#1317),#863,.T.);
#11827=ADVANCED_FACE('',(#1318),#864,.T.);
#11828=ADVANCED_FACE('',(#1319),#865,.T.);
#11829=ADVANCED_FACE('',(#1320),#866,.F.);
#11830=ADVANCED_FACE('',(#1321),#11652,.F.);
#11831=ADVANCED_FACE('',(#1322),#867,.T.);
#11832=ADVANCED_FACE('',(#1323),#11653,.F.);
#11833=ADVANCED_FACE('',(#1324),#868,.T.);
#11834=ADVANCED_FACE('',(#1325),#869,.F.);
#11835=ADVANCED_FACE('',(#1326),#870,.F.);
#11836=ADVANCED_FACE('',(#1327),#871,.F.);
#11837=ADVANCED_FACE('',(#1328),#11654,.F.);
#11838=ADVANCED_FACE('',(#1329),#11655,.T.);
#11839=ADVANCED_FACE('',(#1330),#11656,.T.);
#11840=ADVANCED_FACE('',(#1331,#700,#701),#872,.T.);
#11841=ADVANCED_FACE('',(#1332),#873,.T.);
#11842=ADVANCED_FACE('',(#1333),#874,.T.);
#11843=ADVANCED_FACE('',(#1334),#11657,.F.);
#11844=ADVANCED_FACE('',(#1335),#875,.T.);
#11845=ADVANCED_FACE('',(#1336),#11658,.F.);
#11846=ADVANCED_FACE('',(#1337),#876,.T.);
#11847=ADVANCED_FACE('',(#1338),#877,.F.);
#11848=ADVANCED_FACE('',(#1339),#878,.F.);
#11849=ADVANCED_FACE('',(#1340),#879,.F.);
#11850=ADVANCED_FACE('',(#1341),#11659,.F.);
#11851=ADVANCED_FACE('',(#1342),#11660,.T.);
#11852=ADVANCED_FACE('',(#1343),#11661,.T.);
#11853=ADVANCED_FACE('',(#1344,#702,#703),#880,.T.);
#11854=ADVANCED_FACE('',(#1345),#881,.T.);
#11855=ADVANCED_FACE('',(#1346),#882,.T.);
#11856=ADVANCED_FACE('',(#1347),#11662,.F.);
#11857=ADVANCED_FACE('',(#1348),#11663,.F.);
#11858=ADVANCED_FACE('',(#1349),#11664,.F.);
#11859=ADVANCED_FACE('',(#1350),#11665,.F.);
#11860=ADVANCED_FACE('',(#1351,#704,#705,#706,#707,#708),#883,.T.);
#11861=ADVANCED_FACE('',(#1352),#884,.T.);
#11862=ADVANCED_FACE('',(#1353),#885,.T.);
#11863=ADVANCED_FACE('',(#1354),#886,.T.);
#11864=ADVANCED_FACE('',(#1355),#887,.T.);
#11865=ADVANCED_FACE('',(#1356),#888,.T.);
#11866=ADVANCED_FACE('',(#1357),#889,.T.);
#11867=ADVANCED_FACE('',(#1358),#890,.T.);
#11868=ADVANCED_FACE('',(#1359,#709,#710),#891,.T.);
#11869=ADVANCED_FACE('',(#1360),#892,.T.);
#11870=ADVANCED_FACE('',(#1361,#711,#712,#713,#714),#893,.F.);
#11871=ADVANCED_FACE('',(#1362),#894,.F.);
#11872=ADVANCED_FACE('',(#1363),#895,.F.);
#11873=ADVANCED_FACE('',(#1364),#896,.F.);
#11874=ADVANCED_FACE('',(#1365),#897,.F.);
#11875=ADVANCED_FACE('',(#1366),#898,.F.);
#11876=ADVANCED_FACE('',(#1367),#11666,.F.);
#11877=ADVANCED_FACE('',(#1368),#11667,.T.);
#11878=ADVANCED_FACE('',(#1369),#899,.F.);
#11879=ADVANCED_FACE('',(#1370),#11668,.T.);
#11880=ADVANCED_FACE('',(#1371),#900,.T.);
#11881=ADVANCED_FACE('',(#1372),#11669,.F.);
#11882=ADVANCED_FACE('',(#1373),#11670,.F.);
#11883=ADVANCED_FACE('',(#1374),#901,.F.);
#11884=ADVANCED_FACE('',(#1375),#902,.F.);
#11885=ADVANCED_FACE('',(#1376),#903,.F.);
#11886=ADVANCED_FACE('',(#1377),#904,.F.);
#11887=ADVANCED_FACE('',(#1378),#905,.T.);
#11888=ADVANCED_FACE('',(#1379),#906,.T.);
#11889=ADVANCED_FACE('',(#1380,#715,#716),#907,.T.);
#11890=ADVANCED_FACE('',(#1381),#11671,.F.);
#11891=ADVANCED_FACE('',(#1382),#908,.T.);
#11892=ADVANCED_FACE('',(#1383),#909,.T.);
#11893=ADVANCED_FACE('',(#1384),#910,.T.);
#11894=ADVANCED_FACE('',(#1385,#717,#718),#911,.F.);
#11895=ADVANCED_FACE('',(#1386),#912,.F.);
#11896=ADVANCED_FACE('',(#1387),#913,.F.);
#11897=ADVANCED_FACE('',(#1388),#914,.F.);
#11898=ADVANCED_FACE('',(#1389),#915,.F.);
#11899=ADVANCED_FACE('',(#1390),#916,.F.);
#11900=ADVANCED_FACE('',(#1391),#11672,.F.);
#11901=ADVANCED_FACE('',(#1392),#11673,.T.);
#11902=ADVANCED_FACE('',(#1393),#917,.F.);
#11903=ADVANCED_FACE('',(#1394),#11674,.T.);
#11904=ADVANCED_FACE('',(#1395),#918,.T.);
#11905=ADVANCED_FACE('',(#1396),#11675,.F.);
#11906=ADVANCED_FACE('',(#1397),#11676,.F.);
#11907=ADVANCED_FACE('',(#1398),#919,.F.);
#11908=ADVANCED_FACE('',(#1399),#920,.F.);
#11909=ADVANCED_FACE('',(#1400),#921,.F.);
#11910=ADVANCED_FACE('',(#1401),#922,.F.);
#11911=ADVANCED_FACE('',(#1402),#923,.T.);
#11912=ADVANCED_FACE('',(#1403),#924,.T.);
#11913=ADVANCED_FACE('',(#1404,#719,#720),#925,.T.);
#11914=ADVANCED_FACE('',(#1405),#11677,.F.);
#11915=ADVANCED_FACE('',(#1406),#926,.T.);
#11916=ADVANCED_FACE('',(#1407),#927,.T.);
#11917=ADVANCED_FACE('',(#1408),#928,.T.);
#11918=ADVANCED_FACE('',(#1409,#721,#722),#929,.F.);
#11919=ADVANCED_FACE('',(#1410),#11678,.F.);
#11920=ADVANCED_FACE('',(#1411,#723),#930,.T.);
#11921=ADVANCED_FACE('',(#1412),#11679,.F.);
#11922=ADVANCED_FACE('',(#1413,#724),#931,.T.);
#11923=ADVANCED_FACE('',(#1414),#11680,.F.);
#11924=ADVANCED_FACE('',(#1415),#11681,.F.);
#11925=ADVANCED_FACE('',(#1416),#11682,.T.);
#11926=ADVANCED_FACE('',(#1417,#725,#726),#932,.T.);
#11927=ADVANCED_FACE('',(#1418,#727,#728),#933,.F.);
#11928=ADVANCED_FACE('',(#1419),#11683,.F.);
#11929=ADVANCED_FACE('',(#1420,#729,#730),#934,.F.);
#11930=ADVANCED_FACE('',(#1421),#935,.T.);
#11931=ADVANCED_FACE('',(#1422),#11684,.F.);
#11932=ADVANCED_FACE('',(#1423),#11685,.F.);
#11933=ADVANCED_FACE('',(#1424),#11686,.F.);
#11934=ADVANCED_FACE('',(#1425),#11687,.F.);
#11935=ADVANCED_FACE('',(#1426),#11688,.F.);
#11936=ADVANCED_FACE('',(#1427),#11689,.F.);
#11937=ADVANCED_FACE('',(#1428),#11690,.F.);
#11938=ADVANCED_FACE('',(#1429,#731),#936,.T.);
#11939=ADVANCED_FACE('',(#1430,#732),#937,.T.);
#11940=ADVANCED_FACE('',(#1431),#938,.T.);
#11941=ADVANCED_FACE('',(#1432,#733,#734,#735,#736,#737),#939,.T.);
#11942=ADVANCED_FACE('',(#1433),#940,.T.);
#11943=ADVANCED_FACE('',(#1434,#738,#739,#740,#741,#742),#941,.T.);
#11944=ADVANCED_FACE('',(#1435),#942,.T.);
#11945=ADVANCED_FACE('',(#1436),#943,.T.);
#11946=ADVANCED_FACE('',(#1437),#11691,.F.);
#11947=ADVANCED_FACE('',(#1438),#11692,.F.);
#11948=ADVANCED_FACE('',(#1439),#11693,.F.);
#11949=ADVANCED_FACE('',(#1440),#11694,.F.);
#11950=ADVANCED_FACE('',(#1441),#11695,.F.);
#11951=ADVANCED_FACE('',(#1442),#11696,.T.);
#11952=ADVANCED_FACE('',(#1443,#743),#944,.T.);
#11953=ADVANCED_FACE('',(#1444),#11697,.T.);
#11954=ADVANCED_FACE('',(#1445,#744,#745,#746,#747,#748),#945,.T.);
#11955=ADVANCED_FACE('',(#1446,#749,#750,#751,#752,#753),#946,.F.);
#11956=ADVANCED_FACE('',(#1447),#11698,.F.);
#11957=ADVANCED_FACE('',(#1448),#11699,.F.);
#11958=ADVANCED_FACE('',(#1449),#11700,.F.);
#11959=ADVANCED_FACE('',(#1450),#11701,.F.);
#11960=ADVANCED_FACE('',(#1451),#11702,.F.);
#11961=ADVANCED_FACE('',(#1452),#11703,.T.);
#11962=ADVANCED_FACE('',(#1453,#754),#947,.F.);
#11963=ADVANCED_FACE('',(#1454),#11704,.T.);
#11964=ADVANCED_FACE('',(#1455,#755,#756,#757,#758,#759),#948,.T.);
#11965=ADVANCED_FACE('',(#1456,#760,#761,#762,#763,#764),#949,.F.);
#11966=ADVANCED_FACE('',(#1457),#11705,.F.);
#11967=ADVANCED_FACE('',(#1458,#765,#766),#950,.F.);
#11968=ADVANCED_FACE('',(#1459,#767,#768,#769,#770,#771),#951,.T.);
#11969=ADVANCED_FACE('',(#1460),#11706,.F.);
#11970=ADVANCED_FACE('',(#1461),#11707,.F.);
#11971=ADVANCED_FACE('',(#1462),#11708,.F.);
#11972=ADVANCED_FACE('',(#1463),#11709,.F.);
#11973=ADVANCED_FACE('',(#1464),#11710,.F.);
#11974=ADVANCED_FACE('',(#1465),#11711,.F.);
#11975=ADVANCED_FACE('',(#1466),#11712,.F.);
#11976=ADVANCED_FACE('',(#1467,#772),#952,.T.);
#11977=ADVANCED_FACE('',(#1468,#773),#953,.T.);
#11978=ADVANCED_FACE('',(#1469),#954,.T.);
#11979=ADVANCED_FACE('',(#1470),#955,.T.);
#11980=ADVANCED_FACE('',(#1471),#956,.T.);
#11981=ADVANCED_FACE('',(#1472,#774,#775,#776,#777,#778),#957,.T.);
#11982=ADVANCED_FACE('',(#1473),#958,.T.);
#11983=ADVANCED_FACE('',(#1474),#959,.T.);
#11984=ADVANCED_FACE('',(#1475),#11713,.F.);
#11985=ADVANCED_FACE('',(#1476),#11714,.F.);
#11986=ADVANCED_FACE('',(#1477),#11715,.F.);
#11987=ADVANCED_FACE('',(#1478),#11716,.F.);
#11988=ADVANCED_FACE('',(#1479),#11717,.F.);
#11989=ADVANCED_FACE('',(#1480),#11718,.T.);
#11990=ADVANCED_FACE('',(#1481,#779),#960,.T.);
#11991=ADVANCED_FACE('',(#1482),#11719,.T.);
#11992=ADVANCED_FACE('',(#1483,#780,#781,#782,#783,#784),#961,.T.);
#11993=ADVANCED_FACE('',(#1484,#785,#786,#787,#788,#789),#962,.F.);
#11994=ADVANCED_FACE('',(#1485),#11720,.F.);
#11995=ADVANCED_FACE('',(#1486),#11721,.F.);
#11996=ADVANCED_FACE('',(#1487),#11722,.F.);
#11997=ADVANCED_FACE('',(#1488),#11723,.F.);
#11998=ADVANCED_FACE('',(#1489),#11724,.F.);
#11999=ADVANCED_FACE('',(#1490),#11725,.T.);
#12000=ADVANCED_FACE('',(#1491,#790),#963,.F.);
#12001=ADVANCED_FACE('',(#1492),#11726,.T.);
#12002=ADVANCED_FACE('',(#1493,#791,#792,#793,#794,#795),#964,.T.);
#12003=ADVANCED_FACE('',(#1494,#796,#797,#798,#799,#800),#965,.F.);
#12004=ADVANCED_FACE('',(#1495),#966,.T.);
#12005=ADVANCED_FACE('',(#1496),#477,.T.);
#12006=ADVANCED_FACE('',(#1497),#11727,.T.);
#12007=ADVANCED_FACE('',(#1498),#478,.T.);
#12008=ADVANCED_FACE('',(#1499,#801),#967,.T.);
#12009=ADVANCED_FACE('',(#1500),#479,.T.);
#12010=ADVANCED_FACE('',(#1501),#11728,.T.);
#12011=ADVANCED_FACE('',(#1502),#480,.T.);
#12012=ADVANCED_FACE('',(#1503),#968,.T.);
#12013=ADVANCED_FACE('',(#1504),#969,.F.);
#12014=ADVANCED_FACE('',(#1505),#970,.F.);
#12015=ADVANCED_FACE('',(#1506),#971,.F.);
#12016=ADVANCED_FACE('',(#1507),#972,.F.);
#12017=ADVANCED_FACE('',(#1508),#973,.F.);
#12018=ADVANCED_FACE('',(#1509),#974,.F.);
#12019=ADVANCED_FACE('',(#1510),#975,.F.);
#12020=ADVANCED_FACE('',(#1511),#976,.F.);
#12021=ADVANCED_FACE('',(#1512),#471,.F.);
#12022=ADVANCED_FACE('',(#1513),#11729,.T.);
#12023=ADVANCED_FACE('',(#1514),#11730,.F.);
#12024=ADVANCED_FACE('',(#1515),#481,.F.);
#12025=ADVANCED_FACE('',(#1516,#802),#977,.T.);
#12026=ADVANCED_FACE('',(#1517),#11731,.T.);
#12027=ADVANCED_FACE('',(#1518,#803),#978,.T.);
#12028=ADVANCED_FACE('',(#1519),#482,.F.);
#12029=ADVANCED_FACE('',(#1520),#472,.F.);
#12030=ADVANCED_FACE('',(#1521),#11732,.F.);
#12031=ADVANCED_FACE('',(#1522,#804),#979,.T.);
#12032=ADVANCED_FACE('',(#1523),#483,.T.);
#12033=ADVANCED_FACE('',(#1524),#11733,.T.);
#12034=ADVANCED_FACE('',(#1525),#484,.T.);
#12035=ADVANCED_FACE('',(#1526,#805),#980,.T.);
#12036=ADVANCED_FACE('',(#1527),#11734,.F.);
#12037=ADVANCED_FACE('',(#1528),#457,.T.);
#12038=ADVANCED_FACE('',(#1529),#458,.T.);
#12039=ADVANCED_FACE('',(#1530),#459,.T.);
#12040=ADVANCED_FACE('',(#1531),#460,.T.);
#12041=ADVANCED_FACE('',(#1532),#461,.T.);
#12042=ADVANCED_FACE('',(#1533),#462,.T.);
#12043=ADVANCED_FACE('',(#1534),#463,.T.);
#12044=ADVANCED_FACE('',(#1535),#464,.F.);
#12045=ADVANCED_FACE('',(#1536),#11735,.T.);
#12046=ADVANCED_FACE('',(#1537),#981,.T.);
#12047=ADVANCED_FACE('',(#1538),#465,.F.);
#12048=ADVANCED_FACE('',(#1539),#982,.T.);
#12049=ADVANCED_FACE('',(#1540),#466,.F.);
#12050=ADVANCED_FACE('',(#1541),#983,.T.);
#12051=ADVANCED_FACE('',(#1542),#467,.F.);
#12052=ADVANCED_FACE('',(#1543),#984,.T.);
#12053=ADVANCED_FACE('',(#1544),#468,.F.);
#12054=ADVANCED_FACE('',(#1545),#985,.T.);
#12055=ADVANCED_FACE('',(#1546),#469,.F.);
#12056=ADVANCED_FACE('',(#1547),#11736,.F.);
#12057=ADVANCED_FACE('',(#1548),#986,.T.);
#12058=ADVANCED_FACE('',(#1549),#470,.F.);
#12059=ADVANCED_FACE('',(#1550,#806),#987,.T.);
#12060=ADVANCED_FACE('',(#1551),#988,.T.);
#12061=ADVANCED_FACE('',(#1552,#807),#989,.T.);
#12062=ADVANCED_FACE('',(#1553),#11737,.T.);
#12063=ADVANCED_FACE('',(#1554,#808),#990,.T.);
#12064=ADVANCED_FACE('',(#1555),#11738,.F.);
#12065=ADVANCED_FACE('',(#1556,#809),#991,.T.);
#12066=ADVANCED_FACE('',(#1557),#11739,.T.);
#12067=ADVANCED_FACE('',(#1558,#810),#992,.T.);
#12068=ADVANCED_FACE('',(#1559),#11740,.F.);
#12069=ADVANCED_FACE('',(#1560),#993,.F.);
#12070=ADVANCED_FACE('',(#1561),#994,.F.);
#12071=ADVANCED_FACE('',(#1562),#995,.F.);
#12072=ADVANCED_FACE('',(#1563),#996,.F.);
#12073=ADVANCED_FACE('',(#1564),#997,.F.);
#12074=ADVANCED_FACE('',(#1565),#998,.F.);
#12075=ADVANCED_FACE('',(#1566),#999,.F.);
#12076=ADVANCED_FACE('',(#1567),#1000,.F.);
#12077=ADVANCED_FACE('',(#1568),#1001,.F.);
#12078=ADVANCED_FACE('',(#1569),#1002,.T.);
#12079=ADVANCED_FACE('',(#1570),#485,.T.);
#12080=ADVANCED_FACE('',(#1571),#11741,.T.);
#12081=ADVANCED_FACE('',(#1572),#486,.T.);
#12082=ADVANCED_FACE('',(#1573,#811),#1003,.T.);
#12083=ADVANCED_FACE('',(#1574),#487,.T.);
#12084=ADVANCED_FACE('',(#1575),#11742,.T.);
#12085=ADVANCED_FACE('',(#1576),#11743,.F.);
#12086=ADVANCED_FACE('',(#1577),#1004,.F.);
#12087=ADVANCED_FACE('',(#1578),#1005,.T.);
#12088=ADVANCED_FACE('',(#1579),#1006,.T.);
#12089=ADVANCED_FACE('',(#1580),#1007,.T.);
#12090=ADVANCED_FACE('',(#1581),#1008,.T.);
#12091=ADVANCED_FACE('',(#1582),#1009,.T.);
#12092=ADVANCED_FACE('',(#1583),#1010,.T.);
#12093=ADVANCED_FACE('',(#1584),#1011,.T.);
#12094=ADVANCED_FACE('',(#1585),#1012,.T.);
#12095=ADVANCED_FACE('',(#1586),#1013,.T.);
#12096=ADVANCED_FACE('',(#1587),#1014,.T.);
#12097=ADVANCED_FACE('',(#1588),#1015,.T.);
#12098=ADVANCED_FACE('',(#1589),#1016,.T.);
#12099=ADVANCED_FACE('',(#1590),#1017,.T.);
#12100=ADVANCED_FACE('',(#1591),#1018,.T.);
#12101=ADVANCED_FACE('',(#1592),#1019,.T.);
#12102=ADVANCED_FACE('',(#1593),#1020,.T.);
#12103=ADVANCED_FACE('',(#1594),#1021,.T.);
#12104=ADVANCED_FACE('',(#1595),#1022,.T.);
#12105=ADVANCED_FACE('',(#1596),#1023,.T.);
#12106=ADVANCED_FACE('',(#1597),#1024,.T.);
#12107=ADVANCED_FACE('',(#1598),#1025,.T.);
#12108=ADVANCED_FACE('',(#1599),#1026,.T.);
#12109=ADVANCED_FACE('',(#1600),#1027,.T.);
#12110=ADVANCED_FACE('',(#1601),#1028,.T.);
#12111=ADVANCED_FACE('',(#1602),#1029,.T.);
#12112=ADVANCED_FACE('',(#1603),#1030,.T.);
#12113=ADVANCED_FACE('',(#1604),#1031,.T.);
#12114=ADVANCED_FACE('',(#1605),#1032,.T.);
#12115=ADVANCED_FACE('',(#1606),#1033,.T.);
#12116=ADVANCED_FACE('',(#1607),#1034,.T.);
#12117=ADVANCED_FACE('',(#1608),#1035,.T.);
#12118=ADVANCED_FACE('',(#1609),#1036,.T.);
#12119=ADVANCED_FACE('',(#1610),#1037,.T.);
#12120=ADVANCED_FACE('',(#1611),#1038,.T.);
#12121=ADVANCED_FACE('',(#1612),#1039,.T.);
#12122=ADVANCED_FACE('',(#1613),#1040,.T.);
#12123=ADVANCED_FACE('',(#1614),#1041,.T.);
#12124=ADVANCED_FACE('',(#1615),#1042,.T.);
#12125=ADVANCED_FACE('',(#1616),#1043,.T.);
#12126=ADVANCED_FACE('',(#1617),#1044,.T.);
#12127=ADVANCED_FACE('',(#1618),#1045,.T.);
#12128=ADVANCED_FACE('',(#1619),#1046,.T.);
#12129=ADVANCED_FACE('',(#1620),#1047,.T.);
#12130=ADVANCED_FACE('',(#1621),#1048,.T.);
#12131=ADVANCED_FACE('',(#1622),#1049,.T.);
#12132=ADVANCED_FACE('',(#1623),#1050,.T.);
#12133=ADVANCED_FACE('',(#1624),#1051,.T.);
#12134=ADVANCED_FACE('',(#1625),#1052,.T.);
#12135=ADVANCED_FACE('',(#1626),#1053,.T.);
#12136=ADVANCED_FACE('',(#1627),#1054,.T.);
#12137=ADVANCED_FACE('',(#1628),#1055,.T.);
#12138=ADVANCED_FACE('',(#1629),#1056,.T.);
#12139=ADVANCED_FACE('',(#1630),#1057,.T.);
#12140=ADVANCED_FACE('',(#1631),#1058,.T.);
#12141=ADVANCED_FACE('',(#1632),#1059,.T.);
#12142=ADVANCED_FACE('',(#1633),#1060,.T.);
#12143=ADVANCED_FACE('',(#1634),#1061,.T.);
#12144=ADVANCED_FACE('',(#1635),#1062,.T.);
#12145=ADVANCED_FACE('',(#1636),#1063,.T.);
#12146=ADVANCED_FACE('',(#1637),#1064,.T.);
#12147=ADVANCED_FACE('',(#1638),#1065,.T.);
#12148=ADVANCED_FACE('',(#1639),#1066,.T.);
#12149=ADVANCED_FACE('',(#1640),#1067,.T.);
#12150=ADVANCED_FACE('',(#1641),#1068,.T.);
#12151=ADVANCED_FACE('',(#1642),#1069,.T.);
#12152=ADVANCED_FACE('',(#1643),#1070,.T.);
#12153=ADVANCED_FACE('',(#1644),#1071,.T.);
#12154=ADVANCED_FACE('',(#1645),#1072,.T.);
#12155=ADVANCED_FACE('',(#1646),#1073,.T.);
#12156=ADVANCED_FACE('',(#1647),#1074,.T.);
#12157=ADVANCED_FACE('',(#1648),#1075,.T.);
#12158=ADVANCED_FACE('',(#1649),#1076,.T.);
#12159=ADVANCED_FACE('',(#1650),#1077,.T.);
#12160=ADVANCED_FACE('',(#1651),#1078,.T.);
#12161=ADVANCED_FACE('',(#1652),#1079,.T.);
#12162=ADVANCED_FACE('',(#1653),#1080,.T.);
#12163=ADVANCED_FACE('',(#1654),#1081,.T.);
#12164=ADVANCED_FACE('',(#1655),#1082,.T.);
#12165=ADVANCED_FACE('',(#1656),#1083,.T.);
#12166=ADVANCED_FACE('',(#1657),#1084,.T.);
#12167=ADVANCED_FACE('',(#1658),#1085,.T.);
#12168=ADVANCED_FACE('',(#1659),#1086,.T.);
#12169=ADVANCED_FACE('',(#1660),#1087,.T.);
#12170=ADVANCED_FACE('',(#1661),#1088,.T.);
#12171=ADVANCED_FACE('',(#1662),#1089,.T.);
#12172=ADVANCED_FACE('',(#1663),#1090,.T.);
#12173=ADVANCED_FACE('',(#1664),#1091,.T.);
#12174=ADVANCED_FACE('',(#1665),#1092,.T.);
#12175=ADVANCED_FACE('',(#1666),#1093,.T.);
#12176=ADVANCED_FACE('',(#1667),#1094,.T.);
#12177=ADVANCED_FACE('',(#1668),#1095,.T.);
#12178=ADVANCED_FACE('',(#1669),#1096,.T.);
#12179=ADVANCED_FACE('',(#1670),#1097,.T.);
#12180=ADVANCED_FACE('',(#1671),#1098,.T.);
#12181=ADVANCED_FACE('',(#1672),#1099,.T.);
#12182=ADVANCED_FACE('',(#1673),#1100,.T.);
#12183=ADVANCED_FACE('',(#1674),#1101,.T.);
#12184=ADVANCED_FACE('',(#1675),#1102,.T.);
#12185=ADVANCED_FACE('',(#1676),#1103,.T.);
#12186=ADVANCED_FACE('',(#1677),#1104,.T.);
#12187=ADVANCED_FACE('',(#1678),#1105,.T.);
#12188=ADVANCED_FACE('',(#1679),#1106,.T.);
#12189=ADVANCED_FACE('',(#1680),#1107,.T.);
#12190=ADVANCED_FACE('',(#1681),#1108,.T.);
#12191=ADVANCED_FACE('',(#1682),#1109,.T.);
#12192=ADVANCED_FACE('',(#1683),#1110,.T.);
#12193=ADVANCED_FACE('',(#1684),#1111,.T.);
#12194=ADVANCED_FACE('',(#1685),#1112,.T.);
#12195=ADVANCED_FACE('',(#1686),#1113,.T.);
#12196=ADVANCED_FACE('',(#1687),#1114,.T.);
#12197=ADVANCED_FACE('',(#1688),#1115,.T.);
#12198=ADVANCED_FACE('',(#1689),#1116,.T.);
#12199=ADVANCED_FACE('',(#1690),#1117,.T.);
#12200=ADVANCED_FACE('',(#1691),#1118,.T.);
#12201=ADVANCED_FACE('',(#1692),#1119,.T.);
#12202=ADVANCED_FACE('',(#1693),#1120,.T.);
#12203=ADVANCED_FACE('',(#1694),#1121,.T.);
#12204=ADVANCED_FACE('',(#1695),#1122,.T.);
#12205=ADVANCED_FACE('',(#1696),#1123,.T.);
#12206=ADVANCED_FACE('',(#1697),#1124,.T.);
#12207=ADVANCED_FACE('',(#1698),#1125,.T.);
#12208=ADVANCED_FACE('',(#1699),#1126,.T.);
#12209=ADVANCED_FACE('',(#1700),#1127,.T.);
#12210=ADVANCED_FACE('',(#1701),#1128,.T.);
#12211=ADVANCED_FACE('',(#1702),#1129,.T.);
#12212=ADVANCED_FACE('',(#1703),#1130,.T.);
#12213=ADVANCED_FACE('',(#1704),#1131,.T.);
#12214=ADVANCED_FACE('',(#1705),#1132,.T.);
#12215=ADVANCED_FACE('',(#1706),#1133,.T.);
#12216=ADVANCED_FACE('',(#1707),#1134,.T.);
#12217=ADVANCED_FACE('',(#1708),#1135,.T.);
#12218=ADVANCED_FACE('',(#1709),#1136,.T.);
#12219=ADVANCED_FACE('',(#1710),#1137,.T.);
#12220=ADVANCED_FACE('',(#1711),#1138,.T.);
#12221=ADVANCED_FACE('',(#1712),#1139,.T.);
#12222=ADVANCED_FACE('',(#1713),#1140,.T.);
#12223=ADVANCED_FACE('',(#1714),#1141,.T.);
#12224=ADVANCED_FACE('',(#1715),#1142,.T.);
#12225=ADVANCED_FACE('',(#1716),#1143,.T.);
#12226=ADVANCED_FACE('',(#1717),#1144,.T.);
#12227=ADVANCED_FACE('',(#1718),#1145,.T.);
#12228=ADVANCED_FACE('',(#1719),#1146,.T.);
#12229=ADVANCED_FACE('',(#1720),#1147,.T.);
#12230=ADVANCED_FACE('',(#1721),#1148,.T.);
#12231=ADVANCED_FACE('',(#1722),#1149,.T.);
#12232=ADVANCED_FACE('',(#1723),#1150,.T.);
#12233=ADVANCED_FACE('',(#1724),#1151,.T.);
#12234=ADVANCED_FACE('',(#1725),#1152,.T.);
#12235=ADVANCED_FACE('',(#1726),#1153,.T.);
#12236=ADVANCED_FACE('',(#1727),#1154,.T.);
#12237=ADVANCED_FACE('',(#1728),#1155,.T.);
#12238=ADVANCED_FACE('',(#1729),#1156,.T.);
#12239=ADVANCED_FACE('',(#1730),#1157,.T.);
#12240=ADVANCED_FACE('',(#1731),#1158,.T.);
#12241=ADVANCED_FACE('',(#1732),#1159,.T.);
#12242=ADVANCED_FACE('',(#1733),#1160,.T.);
#12243=ADVANCED_FACE('',(#1734),#1161,.T.);
#12244=ADVANCED_FACE('',(#1735),#1162,.T.);
#12245=ADVANCED_FACE('',(#1736),#1163,.T.);
#12246=ADVANCED_FACE('',(#1737),#1164,.T.);
#12247=ADVANCED_FACE('',(#1738),#1165,.T.);
#12248=ADVANCED_FACE('',(#1739),#1166,.T.);
#12249=ADVANCED_FACE('',(#1740),#1167,.T.);
#12250=ADVANCED_FACE('',(#1741),#1168,.T.);
#12251=ADVANCED_FACE('',(#1742),#1169,.T.);
#12252=ADVANCED_FACE('',(#1743),#1170,.T.);
#12253=ADVANCED_FACE('',(#1744),#1171,.F.);
#12254=ADVANCED_FACE('',(#1745),#11744,.T.);
#12255=ADVANCED_FACE('',(#1746),#1172,.T.);
#12256=ADVANCED_FACE('',(#1747,#812),#1173,.F.);
#12257=ADVANCED_FACE('',(#1748),#11745,.T.);
#12258=ADVANCED_FACE('',(#1749),#1174,.T.);
#12259=ADVANCED_FACE('',(#1750),#11746,.T.);
#12260=ADVANCED_FACE('',(#1751,#813),#1175,.T.);
#12261=ADVANCED_FACE('',(#1752),#1176,.F.);
#12262=ADVANCED_FACE('',(#1753),#11747,.F.);
#12263=ADVANCED_FACE('',(#1754),#1177,.F.);
#12264=ADVANCED_FACE('',(#1755),#1178,.F.);
#12265=ADVANCED_FACE('',(#1756),#1179,.F.);
#12266=ADVANCED_FACE('',(#1757),#1180,.F.);
#12267=ADVANCED_FACE('',(#1758),#1181,.T.);
#12268=ADVANCED_FACE('',(#1759,#814),#11748,.T.);
#12269=ADVANCED_FACE('',(#1760,#815),#11749,.F.);
#12270=ADVANCED_FACE('',(#1761),#1182,.F.);
#12271=ADVANCED_FACE('',(#1762),#1183,.F.);
#12272=ADVANCED_FACE('',(#1763),#1184,.F.);
#12273=ADVANCED_FACE('',(#1764),#1185,.F.);
#12274=ADVANCED_FACE('',(#1765),#1186,.F.);
#12275=ADVANCED_FACE('',(#1766),#1187,.F.);
#12276=ADVANCED_FACE('',(#1767),#1188,.F.);
#12277=ADVANCED_FACE('',(#1768),#1189,.F.);
#12278=ADVANCED_FACE('',(#1769,#816),#1190,.T.);
#12279=ADVANCED_FACE('',(#1770),#488,.T.);
#12280=ADVANCED_FACE('',(#1771),#11750,.T.);
#12281=ADVANCED_FACE('',(#1772),#489,.T.);
#12282=ADVANCED_FACE('',(#1773),#1191,.T.);
#12283=ADVANCED_FACE('',(#1774),#11751,.F.);
#12284=ADVANCED_FACE('',(#1775),#1192,.T.);
#12285=ADVANCED_FACE('',(#1776),#11752,.F.);
#12286=ADVANCED_FACE('',(#1777),#1193,.F.);
#12287=ADVANCED_FACE('',(#1778),#1194,.F.);
#12288=ADVANCED_FACE('',(#1779),#1195,.T.);
#12289=ADVANCED_FACE('',(#1780),#1196,.F.);
#12290=ADVANCED_FACE('',(#1781),#1197,.F.);
#12291=ADVANCED_FACE('',(#1782),#1198,.F.);
#12292=ADVANCED_FACE('',(#1783),#1199,.F.);
#12293=ADVANCED_FACE('',(#1784),#1200,.T.);
#12294=ADVANCED_FACE('',(#1785),#1201,.F.);
#12295=ADVANCED_FACE('',(#1786),#1202,.F.);
#12296=ADVANCED_FACE('',(#1787),#1203,.F.);
#12297=ADVANCED_FACE('',(#1788,#817,#818),#11753,.T.);
#12298=ADVANCED_FACE('',(#1789,#819),#1204,.T.);
#12299=ADVANCED_FACE('',(#1790,#820),#1205,.F.);
#12300=ADVANCED_FACE('',(#1791),#11754,.F.);
#12301=ADVANCED_FACE('',(#1792),#11755,.T.);
#12302=ADVANCED_FACE('',(#1793,#821),#1206,.T.);
#12303=ADVANCED_FACE('',(#1794,#822),#1207,.F.);
#12304=ADVANCED_FACE('',(#1795),#11756,.F.);
#12305=ADVANCED_FACE('',(#1796),#11757,.T.);
#12306=ADVANCED_FACE('',(#1797,#823),#1208,.T.);
#12307=ADVANCED_FACE('',(#1798,#824),#1209,.F.);
#12308=ADVANCED_FACE('',(#1799),#11758,.F.);
#12309=ADVANCED_FACE('',(#1800),#11759,.T.);
#12310=ADVANCED_FACE('',(#1801,#825),#1210,.T.);
#12311=ADVANCED_FACE('',(#1802,#826),#1211,.F.);
#12312=ADVANCED_FACE('',(#1803),#11760,.F.);
#12313=ADVANCED_FACE('',(#1804),#11761,.T.);
#12314=ADVANCED_FACE('',(#1805,#827),#1212,.T.);
#12315=ADVANCED_FACE('',(#1806,#828),#1213,.F.);
#12316=ADVANCED_FACE('',(#1807),#1214,.T.);
#12317=ADVANCED_FACE('',(#1808),#1215,.T.);
#12318=ADVANCED_FACE('',(#1809),#1216,.T.);
#12319=ADVANCED_FACE('',(#1810),#1217,.T.);
#12320=ADVANCED_FACE('',(#1811),#1218,.T.);
#12321=ADVANCED_FACE('',(#1812),#1219,.F.);
#12322=ADVANCED_FACE('',(#1813),#1220,.T.);
#12323=ADVANCED_FACE('',(#1814),#1221,.T.);
#12324=ADVANCED_FACE('',(#1815),#1222,.T.);
#12325=ADVANCED_FACE('',(#1816),#1223,.T.);
#12326=ADVANCED_FACE('',(#1817),#1224,.T.);
#12327=ADVANCED_FACE('',(#1818),#1225,.F.);
#12328=ADVANCED_FACE('',(#1819),#11762,.F.);
#12329=ADVANCED_FACE('',(#1820),#1226,.F.);
#12330=ADVANCED_FACE('',(#1821),#1227,.F.);
#12331=ADVANCED_FACE('',(#1822),#1228,.F.);
#12332=ADVANCED_FACE('',(#1823,#829),#1229,.T.);
#12333=ADVANCED_FACE('',(#1824),#11763,.F.);
#12334=ADVANCED_FACE('',(#1825),#11764,.T.);
#12335=ADVANCED_FACE('',(#1826),#1230,.T.);
#12336=ADVANCED_FACE('',(#1827,#830),#1231,.F.);
#12337=ADVANCED_FACE('',(#1828),#1232,.T.);
#12338=ADVANCED_FACE('',(#1829,#831),#1233,.T.);
#12339=ADVANCED_FACE('',(#1830,#832),#11765,.T.);
#12340=ADVANCED_FACE('',(#1831,#833),#1234,.F.);
#12341=ADVANCED_FACE('',(#1832),#11766,.F.);
#12342=ADVANCED_FACE('',(#1833),#11767,.T.);
#12343=ADVANCED_FACE('',(#1834,#834),#1235,.T.);
#12344=ADVANCED_FACE('',(#1835,#835),#1236,.F.);
#12345=ADVANCED_FACE('',(#1836),#11768,.F.);
#12346=ADVANCED_FACE('',(#1837),#11769,.T.);
#12347=ADVANCED_FACE('',(#1838,#836),#1237,.T.);
#12348=ADVANCED_FACE('',(#1839,#837),#1238,.F.);
#12349=ADVANCED_FACE('',(#1840),#11770,.F.);
#12350=ADVANCED_FACE('',(#1841),#11771,.T.);
#12351=ADVANCED_FACE('',(#1842,#838),#1239,.T.);
#12352=ADVANCED_FACE('',(#1843,#839),#1240,.F.);
#12353=ADVANCED_FACE('',(#1844),#1241,.F.);
#12354=ADVANCED_FACE('',(#1845),#1242,.F.);
#12355=ADVANCED_FACE('',(#1846),#1243,.F.);
#12356=ADVANCED_FACE('',(#1847,#840),#1244,.F.);
#12357=ADVANCED_FACE('',(#1848),#11772,.F.);
#12358=ADVANCED_FACE('',(#1849),#11773,.T.);
#12359=ADVANCED_FACE('',(#1850,#841),#1245,.T.);
#12360=ADVANCED_FACE('',(#1851),#11,.T.);
#12361=ADVANCED_FACE('',(#1852),#1246,.T.);
#12362=ADVANCED_FACE('',(#1853),#12,.T.);
#12363=ADVANCED_FACE('',(#1854),#11774,.T.);
#12364=ADVANCED_FACE('',(#1855),#13,.T.);
#12365=ADVANCED_FACE('',(#1856),#1247,.T.);
#12366=ADVANCED_FACE('',(#1857),#14,.T.);
#12367=ADVANCED_FACE('',(#1858),#11775,.T.);
#12368=ADVANCED_FACE('',(#1859),#15,.T.);
#12369=ADVANCED_FACE('',(#1860),#1248,.T.);
#12370=ADVANCED_FACE('',(#1861),#16,.T.);
#12371=ADVANCED_FACE('',(#1862),#11776,.T.);
#12372=ADVANCED_FACE('',(#1863),#17,.T.);
#12373=ADVANCED_FACE('',(#1864),#1249,.T.);
#12374=ADVANCED_FACE('',(#1865),#18,.T.);
#12375=ADVANCED_FACE('',(#1866),#11777,.T.);
#12376=ADVANCED_FACE('',(#1867),#19,.T.);
#12377=ADVANCED_FACE('',(#1868),#1250,.T.);
#12378=ADVANCED_FACE('',(#1869),#20,.T.);
#12379=ADVANCED_FACE('',(#1870),#11778,.T.);
#12380=ADVANCED_FACE('',(#1871),#21,.T.);
#12381=ADVANCED_FACE('',(#1872),#1251,.T.);
#12382=ADVANCED_FACE('',(#1873),#22,.T.);
#12383=ADVANCED_FACE('',(#1874),#11779,.T.);
#12384=ADVANCED_FACE('',(#1875),#23,.T.);
#12385=ADVANCED_FACE('',(#1876),#1252,.T.);
#12386=ADVANCED_FACE('',(#1877),#24,.T.);
#12387=ADVANCED_FACE('',(#1878),#11780,.T.);
#12388=ADVANCED_FACE('',(#1879),#25,.T.);
#12389=ADVANCED_FACE('',(#1880),#1253,.T.);
#12390=ADVANCED_FACE('',(#1881),#26,.T.);
#12391=ADVANCED_FACE('',(#1882),#11781,.T.);
#12392=ADVANCED_FACE('',(#1883),#27,.T.);
#12393=ADVANCED_FACE('',(#1884),#1254,.T.);
#12394=ADVANCED_FACE('',(#1885),#28,.T.);
#12395=ADVANCED_FACE('',(#1886),#11782,.T.);
#12396=ADVANCED_FACE('',(#1887),#29,.T.);
#12397=ADVANCED_FACE('',(#1888),#1255,.T.);
#12398=ADVANCED_FACE('',(#1889),#30,.T.);
#12399=ADVANCED_FACE('',(#1890),#11783,.T.);
#12400=ADVANCED_FACE('',(#1891),#31,.T.);
#12401=ADVANCED_FACE('',(#1892),#1256,.T.);
#12402=ADVANCED_FACE('',(#1893),#32,.T.);
#12403=ADVANCED_FACE('',(#1894),#11784,.T.);
#12404=ADVANCED_FACE('',(#1895),#33,.T.);
#12405=ADVANCED_FACE('',(#1896),#1257,.T.);
#12406=ADVANCED_FACE('',(#1897),#34,.T.);
#12407=ADVANCED_FACE('',(#1898),#11785,.T.);
#12408=ADVANCED_FACE('',(#1899),#35,.T.);
#12409=ADVANCED_FACE('',(#1900),#1258,.T.);
#12410=ADVANCED_FACE('',(#1901),#36,.T.);
#12411=ADVANCED_FACE('',(#1902),#11786,.T.);
#12412=ADVANCED_FACE('',(#1903),#37,.T.);
#12413=ADVANCED_FACE('',(#1904),#1259,.T.);
#12414=ADVANCED_FACE('',(#1905),#38,.T.);
#12415=ADVANCED_FACE('',(#1906),#11787,.T.);
#12416=ADVANCED_FACE('',(#1907),#39,.T.);
#12417=ADVANCED_FACE('',(#1908),#1260,.T.);
#12418=ADVANCED_FACE('',(#1909),#40,.T.);
#12419=ADVANCED_FACE('',(#1910),#11788,.T.);
#12420=ADVANCED_FACE('',(#1911),#41,.T.);
#12421=ADVANCED_FACE('',(#1912),#1261,.T.);
#12422=ADVANCED_FACE('',(#1913),#42,.T.);
#12423=ADVANCED_FACE('',(#1914),#11789,.T.);
#12424=ADVANCED_FACE('',(#1915),#43,.T.);
#12425=ADVANCED_FACE('',(#1916),#1262,.T.);
#12426=ADVANCED_FACE('',(#1917),#44,.T.);
#12427=ADVANCED_FACE('',(#1918),#11790,.T.);
#12428=ADVANCED_FACE('',(#1919),#45,.T.);
#12429=ADVANCED_FACE('',(#1920),#1263,.T.);
#12430=ADVANCED_FACE('',(#1921),#46,.T.);
#12431=ADVANCED_FACE('',(#1922),#11791,.T.);
#12432=ADVANCED_FACE('',(#1923),#47,.T.);
#12433=ADVANCED_FACE('',(#1924),#1264,.T.);
#12434=ADVANCED_FACE('',(#1925),#48,.T.);
#12435=ADVANCED_FACE('',(#1926),#11792,.T.);
#12436=ADVANCED_FACE('',(#1927),#49,.T.);
#12437=ADVANCED_FACE('',(#1928),#1265,.T.);
#12438=ADVANCED_FACE('',(#1929),#50,.T.);
#12439=ADVANCED_FACE('',(#1930,#842),#1266,.T.);
#12440=ADVANCED_FACE('',(#1931),#11793,.T.);
#12441=ADVANCED_FACE('',(#1932),#11794,.F.);
#12442=ADVANCED_FACE('',(#1933),#11795,.T.);
#12443=ADVANCED_FACE('',(#1934,#843),#1267,.T.);
#12444=ADVANCED_FACE('',(#1935,#844),#1268,.F.);
#12445=ADVANCED_FACE('',(#1936),#1269,.T.);
#12446=ADVANCED_FACE('',(#1937),#490,.T.);
#12447=ADVANCED_FACE('',(#1938),#11796,.T.);
#12448=ADVANCED_FACE('',(#1939),#491,.T.);
#12449=ADVANCED_FACE('',(#1940,#845),#1270,.T.);
#12450=ADVANCED_FACE('',(#1941),#492,.T.);
#12451=ADVANCED_FACE('',(#1942),#11797,.T.);
#12452=ADVANCED_FACE('',(#1943),#493,.T.);
#12453=ADVANCED_FACE('',(#1944),#1271,.T.);
#12454=ADVANCED_FACE('',(#1945),#1272,.F.);
#12455=ADVANCED_FACE('',(#1946),#1273,.F.);
#12456=ADVANCED_FACE('',(#1947),#1274,.F.);
#12457=ADVANCED_FACE('',(#1948),#1275,.F.);
#12458=ADVANCED_FACE('',(#1949),#1276,.F.);
#12459=ADVANCED_FACE('',(#1950),#1277,.F.);
#12460=ADVANCED_FACE('',(#1951),#1278,.F.);
#12461=ADVANCED_FACE('',(#1952),#1279,.F.);
#12462=ADVANCED_FACE('',(#1953),#1280,.T.);
#12463=ADVANCED_FACE('',(#1954),#494,.T.);
#12464=ADVANCED_FACE('',(#1955),#11798,.T.);
#12465=ADVANCED_FACE('',(#1956),#495,.T.);
#12466=ADVANCED_FACE('',(#1957,#846),#1281,.T.);
#12467=ADVANCED_FACE('',(#1958),#496,.T.);
#12468=ADVANCED_FACE('',(#1959),#11799,.T.);
#12469=ADVANCED_FACE('',(#1960),#497,.T.);
#12470=ADVANCED_FACE('',(#1961),#1282,.T.);
#12471=ADVANCED_FACE('',(#1962),#1283,.F.);
#12472=ADVANCED_FACE('',(#1963),#1284,.F.);
#12473=ADVANCED_FACE('',(#1964),#1285,.F.);
#12474=ADVANCED_FACE('',(#1965),#1286,.F.);
#12475=ADVANCED_FACE('',(#1966),#1287,.F.);
#12476=ADVANCED_FACE('',(#1967),#1288,.F.);
#12477=ADVANCED_FACE('',(#1968),#1289,.F.);
#12478=ADVANCED_FACE('',(#1969),#1290,.F.);
#12479=ADVANCED_FACE('',(#1970),#11800,.F.);
#12480=ADVANCED_FACE('',(#1971),#11801,.T.);
#12481=ADVANCED_FACE('',(#1972,#847),#1291,.T.);
#12482=ADVANCED_FACE('',(#1973,#848),#1292,.F.);
#12483=CLOSED_SHELL('',(#11802,#11803,#11804,#11805,#11806,#11807,#11808,
#11809,#11810,#11811,#11812,#11813,#11814,#11815,#11816,#11817));
#12484=CLOSED_SHELL('',(#11818,#11819,#11820,#11821,#11822,#11823));
#12485=CLOSED_SHELL('',(#11824,#11825,#11826,#11827,#11828,#11829));
#12486=CLOSED_SHELL('',(#11830,#11831,#11832,#11833,#11834,#11835,#11836,
#11837,#11838,#11839,#11840,#11841,#11842,#11843,#11844,#11845,#11846,#11847,
#11848,#11849,#11850,#11851,#11852,#11853,#11854,#11855,#11856,#11857,#11858,
#11859,#11860,#11861,#11862,#11863,#11864,#11865,#11866,#11867,#11868,#11869,
#11870));
#12487=CLOSED_SHELL('',(#11871,#11872,#11873,#11874,#11875,#11876,#11877,
#11878,#11879,#11880));
#12488=CLOSED_SHELL('',(#11881,#11882,#11883,#11884,#11885,#11886,#11887,
#11888,#11889,#11890,#11891,#11892,#11893,#11894));
#12489=CLOSED_SHELL('',(#11895,#11896,#11897,#11898,#11899,#11900,#11901,
#11902,#11903,#11904));
#12490=CLOSED_SHELL('',(#11905,#11906,#11907,#11908,#11909,#11910,#11911,
#11912,#11913,#11914,#11915,#11916,#11917,#11918));
#12491=CLOSED_SHELL('',(#11919,#11920,#11921,#11922,#11923,#11924,#11925,
#11926,#11927));
#12492=CLOSED_SHELL('',(#11928,#11929,#11930,#11931,#11932,#11933,#11934,
#11935,#11936,#11937,#11938,#11939,#11940,#11941,#11942,#11943,#11944,#11945));
#12493=CLOSED_SHELL('',(#11946,#11947,#11948,#11949,#11950,#11951,#11952,
#11953,#11954,#11955));
#12494=CLOSED_SHELL('',(#11956,#11957,#11958,#11959,#11960,#11961,#11962,
#11963,#11964,#11965));
#12495=CLOSED_SHELL('',(#11966,#11967,#11968,#11969,#11970,#11971,#11972,
#11973,#11974,#11975,#11976,#11977,#11978,#11979,#11980,#11981,#11982,#11983));
#12496=CLOSED_SHELL('',(#11984,#11985,#11986,#11987,#11988,#11989,#11990,
#11991,#11992,#11993));
#12497=CLOSED_SHELL('',(#11994,#11995,#11996,#11997,#11998,#11999,#12000,
#12001,#12002,#12003));
#12498=CLOSED_SHELL('',(#12004,#12005,#12006,#12007,#12008,#12009,#12010,
#12011,#12012));
#12499=CLOSED_SHELL('',(#12013,#12014,#12015,#12016,#12017,#12018,#12019,
#12020));
#12500=CLOSED_SHELL('',(#12021,#12022,#12023,#12024,#12025,#12026,#12027,
#12028));
#12501=CLOSED_SHELL('',(#12029,#12030,#12031,#12032,#12033,#12034,#12035,
#12036));
#12502=CLOSED_SHELL('',(#12037));
#12503=CLOSED_SHELL('',(#12038));
#12504=CLOSED_SHELL('',(#12039));
#12505=CLOSED_SHELL('',(#12040));
#12506=CLOSED_SHELL('',(#12041));
#12507=CLOSED_SHELL('',(#12042));
#12508=CLOSED_SHELL('',(#12043));
#12509=CLOSED_SHELL('',(#12044,#12045,#12046,#12047,#12048,#12049,#12050,
#12051,#12052,#12053,#12054,#12055,#12056,#12057,#12058,#12059,#12060));
#12510=CLOSED_SHELL('',(#12061,#12062,#12063,#12064));
#12511=CLOSED_SHELL('',(#12065,#12066,#12067,#12068));
#12512=CLOSED_SHELL('',(#12069,#12070,#12071,#12072,#12073,#12074,#12075,
#12076));
#12513=CLOSED_SHELL('',(#12077,#12078,#12079,#12080,#12081,#12082,#12083,
#12084));
#12514=CLOSED_SHELL('',(#12085,#12086,#12087,#12088,#12089,#12090,#12091,
#12092,#12093,#12094,#12095,#12096,#12097,#12098,#12099,#12100,#12101,#12102,
#12103,#12104,#12105,#12106,#12107,#12108,#12109,#12110,#12111,#12112,#12113,
#12114,#12115,#12116,#12117,#12118,#12119,#12120,#12121,#12122,#12123,#12124,
#12125,#12126,#12127,#12128,#12129,#12130,#12131,#12132,#12133,#12134,#12135,
#12136,#12137,#12138,#12139,#12140,#12141,#12142,#12143,#12144,#12145,#12146,
#12147,#12148,#12149,#12150,#12151,#12152,#12153,#12154,#12155,#12156,#12157,
#12158,#12159,#12160,#12161,#12162,#12163,#12164,#12165,#12166,#12167,#12168,
#12169,#12170,#12171,#12172,#12173,#12174,#12175,#12176,#12177,#12178,#12179,
#12180,#12181,#12182,#12183,#12184,#12185,#12186,#12187,#12188,#12189,#12190,
#12191,#12192,#12193,#12194,#12195,#12196,#12197,#12198,#12199,#12200,#12201,
#12202,#12203,#12204,#12205,#12206,#12207,#12208,#12209,#12210,#12211,#12212,
#12213,#12214,#12215,#12216,#12217,#12218,#12219,#12220,#12221,#12222,#12223,
#12224,#12225,#12226,#12227,#12228,#12229,#12230,#12231,#12232,#12233,#12234,
#12235,#12236,#12237,#12238,#12239,#12240,#12241,#12242,#12243,#12244,#12245,
#12246,#12247,#12248,#12249,#12250,#12251,#12252,#12253,#12254,#12255,#12256));
#12515=CLOSED_SHELL('',(#12257,#12258,#12259,#12260,#12261));
#12516=CLOSED_SHELL('',(#12262,#12263,#12264,#12265,#12266,#12267,#12268,
#12269,#12270));
#12517=CLOSED_SHELL('',(#12271,#12272,#12273,#12274,#12275,#12276,#12277,
#12278,#12279,#12280,#12281,#12282));
#12518=CLOSED_SHELL('',(#12283,#12284,#12285,#12286,#12287,#12288,#12289,
#12290,#12291,#12292,#12293,#12294,#12295,#12296,#12297,#12298,#12299));
#12519=CLOSED_SHELL('',(#12300,#12301,#12302,#12303));
#12520=CLOSED_SHELL('',(#12304,#12305,#12306,#12307));
#12521=CLOSED_SHELL('',(#12308,#12309,#12310,#12311));
#12522=CLOSED_SHELL('',(#12312,#12313,#12314,#12315));
#12523=CLOSED_SHELL('',(#12316,#12317,#12318,#12319,#12320,#12321));
#12524=CLOSED_SHELL('',(#12322,#12323,#12324,#12325,#12326,#12327));
#12525=CLOSED_SHELL('',(#12328,#12329,#12330,#12331,#12332,#12333,#12334,
#12335,#12336,#12337,#12338,#12339,#12340));
#12526=CLOSED_SHELL('',(#12341,#12342,#12343,#12344));
#12527=CLOSED_SHELL('',(#12345,#12346,#12347,#12348));
#12528=CLOSED_SHELL('',(#12349,#12350,#12351,#12352));
#12529=CLOSED_SHELL('',(#12353,#12354,#12355,#12356,#12357,#12358,#12359,
#12360,#12361,#12362,#12363,#12364,#12365,#12366,#12367,#12368,#12369,#12370,
#12371,#12372,#12373,#12374,#12375,#12376,#12377,#12378,#12379,#12380,#12381,
#12382,#12383,#12384,#12385,#12386,#12387,#12388,#12389,#12390,#12391,#12392,
#12393,#12394,#12395,#12396,#12397,#12398,#12399,#12400,#12401,#12402,#12403,
#12404,#12405,#12406,#12407,#12408,#12409,#12410,#12411,#12412,#12413,#12414,
#12415,#12416,#12417,#12418,#12419,#12420,#12421,#12422,#12423,#12424,#12425,
#12426,#12427,#12428,#12429,#12430,#12431,#12432,#12433,#12434,#12435,#12436,
#12437,#12438,#12439,#12440));
#12530=CLOSED_SHELL('',(#12441,#12442,#12443,#12444));
#12531=CLOSED_SHELL('',(#12445,#12446,#12447,#12448,#12449,#12450,#12451,
#12452,#12453));
#12532=CLOSED_SHELL('',(#12454,#12455,#12456,#12457,#12458,#12459,#12460,
#12461));
#12533=CLOSED_SHELL('',(#12462,#12463,#12464,#12465,#12466,#12467,#12468,
#12469,#12470));
#12534=CLOSED_SHELL('',(#12471,#12472,#12473,#12474,#12475,#12476,#12477,
#12478));
#12535=CLOSED_SHELL('',(#12479,#12480,#12481,#12482));
#12536=DERIVED_UNIT_ELEMENT(#12620,1.);
#12537=DERIVED_UNIT_ELEMENT(#32753,-3.);
#12538=DERIVED_UNIT_ELEMENT(#12620,1.);
#12539=DERIVED_UNIT_ELEMENT(#32753,-3.);
#12540=DERIVED_UNIT_ELEMENT(#12620,1.);
#12541=DERIVED_UNIT_ELEMENT(#32753,-3.);
#12542=DERIVED_UNIT_ELEMENT(#12620,1.);
#12543=DERIVED_UNIT_ELEMENT(#32753,-3.);
#12544=DERIVED_UNIT_ELEMENT(#12620,1.);
#12545=DERIVED_UNIT_ELEMENT(#32753,-3.);
#12546=DERIVED_UNIT_ELEMENT(#12620,1.);
#12547=DERIVED_UNIT_ELEMENT(#32753,-3.);
#12548=DERIVED_UNIT_ELEMENT(#12620,1.);
#12549=DERIVED_UNIT_ELEMENT(#32753,-3.);
#12550=DERIVED_UNIT_ELEMENT(#12620,1.);
#12551=DERIVED_UNIT_ELEMENT(#32753,-3.);
#12552=DERIVED_UNIT_ELEMENT(#12620,1.);
#12553=DERIVED_UNIT_ELEMENT(#32753,-3.);
#12554=DERIVED_UNIT_ELEMENT(#12620,1.);
#12555=DERIVED_UNIT_ELEMENT(#32753,-3.);
#12556=DERIVED_UNIT_ELEMENT(#12620,1.);
#12557=DERIVED_UNIT_ELEMENT(#32753,-3.);
#12558=DERIVED_UNIT_ELEMENT(#12620,1.);
#12559=DERIVED_UNIT_ELEMENT(#32753,-3.);
#12560=DERIVED_UNIT_ELEMENT(#12620,1.);
#12561=DERIVED_UNIT_ELEMENT(#32753,-3.);
#12562=DERIVED_UNIT_ELEMENT(#12620,1.);
#12563=DERIVED_UNIT_ELEMENT(#32753,-3.);
#12564=DERIVED_UNIT_ELEMENT(#12620,1.);
#12565=DERIVED_UNIT_ELEMENT(#32753,-3.);
#12566=DERIVED_UNIT_ELEMENT(#12620,1.);
#12567=DERIVED_UNIT_ELEMENT(#32753,-3.);
#12568=DERIVED_UNIT_ELEMENT(#12620,1.);
#12569=DERIVED_UNIT_ELEMENT(#32753,-3.);
#12570=DERIVED_UNIT_ELEMENT(#12620,1.);
#12571=DERIVED_UNIT_ELEMENT(#32753,-3.);
#12572=DERIVED_UNIT_ELEMENT(#12620,1.);
#12573=DERIVED_UNIT_ELEMENT(#32753,-3.);
#12574=DERIVED_UNIT_ELEMENT(#12620,1.);
#12575=DERIVED_UNIT_ELEMENT(#32753,-3.);
#12576=DERIVED_UNIT_ELEMENT(#12620,1.);
#12577=DERIVED_UNIT_ELEMENT(#32753,-3.);
#12578=DERIVED_UNIT_ELEMENT(#12620,1.);
#12579=DERIVED_UNIT_ELEMENT(#32753,-3.);
#12580=DERIVED_UNIT_ELEMENT(#12620,1.);
#12581=DERIVED_UNIT_ELEMENT(#32753,-3.);
#12582=DERIVED_UNIT_ELEMENT(#12620,1.);
#12583=DERIVED_UNIT_ELEMENT(#32753,-3.);
#12584=DERIVED_UNIT_ELEMENT(#12620,1.);
#12585=DERIVED_UNIT_ELEMENT(#32753,-3.);
#12586=DERIVED_UNIT_ELEMENT(#12620,1.);
#12587=DERIVED_UNIT_ELEMENT(#32753,-3.);
#12588=DERIVED_UNIT_ELEMENT(#12620,1.);
#12589=DERIVED_UNIT_ELEMENT(#32753,-3.);
#12590=DERIVED_UNIT_ELEMENT(#12620,1.);
#12591=DERIVED_UNIT_ELEMENT(#32753,-3.);
#12592=DERIVED_UNIT_ELEMENT(#12620,1.);
#12593=DERIVED_UNIT_ELEMENT(#32753,-3.);
#12594=DERIVED_UNIT_ELEMENT(#12620,1.);
#12595=DERIVED_UNIT_ELEMENT(#32753,-3.);
#12596=DERIVED_UNIT_ELEMENT(#12620,1.);
#12597=DERIVED_UNIT_ELEMENT(#32753,-3.);
#12598=DERIVED_UNIT_ELEMENT(#12620,1.);
#12599=DERIVED_UNIT_ELEMENT(#32753,-3.);
#12600=DERIVED_UNIT_ELEMENT(#12620,1.);
#12601=DERIVED_UNIT_ELEMENT(#32753,-3.);
#12602=DERIVED_UNIT_ELEMENT(#12620,1.);
#12603=DERIVED_UNIT_ELEMENT(#32753,-3.);
#12604=DERIVED_UNIT_ELEMENT(#12620,1.);
#12605=DERIVED_UNIT_ELEMENT(#32753,-3.);
#12606=DERIVED_UNIT_ELEMENT(#12620,1.);
#12607=DERIVED_UNIT_ELEMENT(#32753,-3.);
#12608=DERIVED_UNIT_ELEMENT(#12620,1.);
#12609=DERIVED_UNIT_ELEMENT(#32753,-3.);
#12610=DERIVED_UNIT_ELEMENT(#12620,1.);
#12611=DERIVED_UNIT_ELEMENT(#32753,-3.);
#12612=DERIVED_UNIT_ELEMENT(#12620,1.);
#12613=DERIVED_UNIT_ELEMENT(#32753,-3.);
#12614=DERIVED_UNIT_ELEMENT(#12620,1.);
#12615=DERIVED_UNIT_ELEMENT(#32753,-3.);
#12616=DERIVED_UNIT_ELEMENT(#12620,1.);
#12617=DERIVED_UNIT_ELEMENT(#32753,-3.);
#12618=DERIVED_UNIT_ELEMENT(#12620,1.);
#12619=DERIVED_UNIT_ELEMENT(#32753,-3.);
#12620=(
MASS_UNIT()
NAMED_UNIT(*)
SI_UNIT(.KILO.,.GRAM.)
);
#12621=DERIVED_UNIT((#12536,#12537));
#12622=DERIVED_UNIT((#12538,#12539));
#12623=DERIVED_UNIT((#12540,#12541));
#12624=DERIVED_UNIT((#12542,#12543));
#12625=DERIVED_UNIT((#12544,#12545));
#12626=DERIVED_UNIT((#12546,#12547));
#12627=DERIVED_UNIT((#12548,#12549));
#12628=DERIVED_UNIT((#12550,#12551));
#12629=DERIVED_UNIT((#12552,#12553));
#12630=DERIVED_UNIT((#12554,#12555));
#12631=DERIVED_UNIT((#12556,#12557));
#12632=DERIVED_UNIT((#12558,#12559));
#12633=DERIVED_UNIT((#12560,#12561));
#12634=DERIVED_UNIT((#12562,#12563));
#12635=DERIVED_UNIT((#12564,#12565));
#12636=DERIVED_UNIT((#12566,#12567));
#12637=DERIVED_UNIT((#12568,#12569));
#12638=DERIVED_UNIT((#12570,#12571));
#12639=DERIVED_UNIT((#12572,#12573));
#12640=DERIVED_UNIT((#12574,#12575));
#12641=DERIVED_UNIT((#12576,#12577));
#12642=DERIVED_UNIT((#12578,#12579));
#12643=DERIVED_UNIT((#12580,#12581));
#12644=DERIVED_UNIT((#12582,#12583));
#12645=DERIVED_UNIT((#12584,#12585));
#12646=DERIVED_UNIT((#12586,#12587));
#12647=DERIVED_UNIT((#12588,#12589));
#12648=DERIVED_UNIT((#12590,#12591));
#12649=DERIVED_UNIT((#12592,#12593));
#12650=DERIVED_UNIT((#12594,#12595));
#12651=DERIVED_UNIT((#12596,#12597));
#12652=DERIVED_UNIT((#12598,#12599));
#12653=DERIVED_UNIT((#12600,#12601));
#12654=DERIVED_UNIT((#12602,#12603));
#12655=DERIVED_UNIT((#12604,#12605));
#12656=DERIVED_UNIT((#12606,#12607));
#12657=DERIVED_UNIT((#12608,#12609));
#12658=DERIVED_UNIT((#12610,#12611));
#12659=DERIVED_UNIT((#12612,#12613));
#12660=DERIVED_UNIT((#12614,#12615));
#12661=DERIVED_UNIT((#12616,#12617));
#12662=DERIVED_UNIT((#12618,#12619));
#12663=MEASURE_REPRESENTATION_ITEM('density measure',
POSITIVE_RATIO_MEASURE(7850.),#12621);
#12664=MEASURE_REPRESENTATION_ITEM('density measure',
POSITIVE_RATIO_MEASURE(7850.),#12622);
#12665=MEASURE_REPRESENTATION_ITEM('density measure',
POSITIVE_RATIO_MEASURE(7850.),#12623);
#12666=MEASURE_REPRESENTATION_ITEM('density measure',
POSITIVE_RATIO_MEASURE(7850.),#12624);
#12667=MEASURE_REPRESENTATION_ITEM('density measure',
POSITIVE_RATIO_MEASURE(7850.),#12625);
#12668=MEASURE_REPRESENTATION_ITEM('density measure',
POSITIVE_RATIO_MEASURE(7850.),#12626);
#12669=MEASURE_REPRESENTATION_ITEM('density measure',
POSITIVE_RATIO_MEASURE(7850.),#12627);
#12670=MEASURE_REPRESENTATION_ITEM('density measure',
POSITIVE_RATIO_MEASURE(7850.),#12628);
#12671=MEASURE_REPRESENTATION_ITEM('density measure',
POSITIVE_RATIO_MEASURE(7850.),#12629);
#12672=MEASURE_REPRESENTATION_ITEM('density measure',
POSITIVE_RATIO_MEASURE(7850.),#12630);
#12673=MEASURE_REPRESENTATION_ITEM('density measure',
POSITIVE_RATIO_MEASURE(7850.),#12631);
#12674=MEASURE_REPRESENTATION_ITEM('density measure',
POSITIVE_RATIO_MEASURE(7850.),#12632);
#12675=MEASURE_REPRESENTATION_ITEM('density measure',
POSITIVE_RATIO_MEASURE(7850.),#12633);
#12676=MEASURE_REPRESENTATION_ITEM('density measure',
POSITIVE_RATIO_MEASURE(7850.),#12634);
#12677=MEASURE_REPRESENTATION_ITEM('density measure',
POSITIVE_RATIO_MEASURE(7850.),#12635);
#12678=MEASURE_REPRESENTATION_ITEM('density measure',
POSITIVE_RATIO_MEASURE(7850.),#12636);
#12679=MEASURE_REPRESENTATION_ITEM('density measure',
POSITIVE_RATIO_MEASURE(7850.),#12637);
#12680=MEASURE_REPRESENTATION_ITEM('density measure',
POSITIVE_RATIO_MEASURE(7850.),#12638);
#12681=MEASURE_REPRESENTATION_ITEM('density measure',
POSITIVE_RATIO_MEASURE(7850.),#12639);
#12682=MEASURE_REPRESENTATION_ITEM('density measure',
POSITIVE_RATIO_MEASURE(7850.),#12640);
#12683=MEASURE_REPRESENTATION_ITEM('density measure',
POSITIVE_RATIO_MEASURE(7850.),#12641);
#12684=MEASURE_REPRESENTATION_ITEM('density measure',
POSITIVE_RATIO_MEASURE(7850.),#12642);
#12685=MEASURE_REPRESENTATION_ITEM('density measure',
POSITIVE_RATIO_MEASURE(7850.),#12643);
#12686=MEASURE_REPRESENTATION_ITEM('density measure',
POSITIVE_RATIO_MEASURE(7850.),#12644);
#12687=MEASURE_REPRESENTATION_ITEM('density measure',
POSITIVE_RATIO_MEASURE(7850.),#12645);
#12688=MEASURE_REPRESENTATION_ITEM('density measure',
POSITIVE_RATIO_MEASURE(7850.),#12646);
#12689=MEASURE_REPRESENTATION_ITEM('density measure',
POSITIVE_RATIO_MEASURE(7850.),#12647);
#12690=MEASURE_REPRESENTATION_ITEM('density measure',
POSITIVE_RATIO_MEASURE(7850.),#12648);
#12691=MEASURE_REPRESENTATION_ITEM('density measure',
POSITIVE_RATIO_MEASURE(7850.),#12649);
#12692=MEASURE_REPRESENTATION_ITEM('density measure',
POSITIVE_RATIO_MEASURE(7850.),#12650);
#12693=MEASURE_REPRESENTATION_ITEM('density measure',
POSITIVE_RATIO_MEASURE(7850.),#12651);
#12694=MEASURE_REPRESENTATION_ITEM('density measure',
POSITIVE_RATIO_MEASURE(7850.),#12652);
#12695=MEASURE_REPRESENTATION_ITEM('density measure',
POSITIVE_RATIO_MEASURE(7850.),#12653);
#12696=MEASURE_REPRESENTATION_ITEM('density measure',
POSITIVE_RATIO_MEASURE(7850.),#12654);
#12697=MEASURE_REPRESENTATION_ITEM('density measure',
POSITIVE_RATIO_MEASURE(7850.),#12655);
#12698=MEASURE_REPRESENTATION_ITEM('density measure',
POSITIVE_RATIO_MEASURE(7850.),#12656);
#12699=MEASURE_REPRESENTATION_ITEM('density measure',
POSITIVE_RATIO_MEASURE(7850.),#12657);
#12700=MEASURE_REPRESENTATION_ITEM('density measure',
POSITIVE_RATIO_MEASURE(7850.),#12658);
#12701=MEASURE_REPRESENTATION_ITEM('density measure',
POSITIVE_RATIO_MEASURE(7850.),#12659);
#12702=MEASURE_REPRESENTATION_ITEM('density measure',
POSITIVE_RATIO_MEASURE(7850.),#12660);
#12703=MEASURE_REPRESENTATION_ITEM('density measure',
POSITIVE_RATIO_MEASURE(7850.),#12661);
#12704=MEASURE_REPRESENTATION_ITEM('density measure',
POSITIVE_RATIO_MEASURE(7850.),#12662);
#12705=PROPERTY_DEFINITION_REPRESENTATION(#12915,#12789);
#12706=PROPERTY_DEFINITION_REPRESENTATION(#12916,#12790);
#12707=PROPERTY_DEFINITION_REPRESENTATION(#12917,#12791);
#12708=PROPERTY_DEFINITION_REPRESENTATION(#12918,#12792);
#12709=PROPERTY_DEFINITION_REPRESENTATION(#12919,#12793);
#12710=PROPERTY_DEFINITION_REPRESENTATION(#12920,#12794);
#12711=PROPERTY_DEFINITION_REPRESENTATION(#12921,#12795);
#12712=PROPERTY_DEFINITION_REPRESENTATION(#12922,#12796);
#12713=PROPERTY_DEFINITION_REPRESENTATION(#12923,#12797);
#12714=PROPERTY_DEFINITION_REPRESENTATION(#12924,#12798);
#12715=PROPERTY_DEFINITION_REPRESENTATION(#12925,#12799);
#12716=PROPERTY_DEFINITION_REPRESENTATION(#12926,#12800);
#12717=PROPERTY_DEFINITION_REPRESENTATION(#12927,#12801);
#12718=PROPERTY_DEFINITION_REPRESENTATION(#12928,#12802);
#12719=PROPERTY_DEFINITION_REPRESENTATION(#12929,#12803);
#12720=PROPERTY_DEFINITION_REPRESENTATION(#12930,#12804);
#12721=PROPERTY_DEFINITION_REPRESENTATION(#12931,#12805);
#12722=PROPERTY_DEFINITION_REPRESENTATION(#12932,#12806);
#12723=PROPERTY_DEFINITION_REPRESENTATION(#12933,#12807);
#12724=PROPERTY_DEFINITION_REPRESENTATION(#12934,#12808);
#12725=PROPERTY_DEFINITION_REPRESENTATION(#12935,#12809);
#12726=PROPERTY_DEFINITION_REPRESENTATION(#12936,#12810);
#12727=PROPERTY_DEFINITION_REPRESENTATION(#12937,#12811);
#12728=PROPERTY_DEFINITION_REPRESENTATION(#12938,#12812);
#12729=PROPERTY_DEFINITION_REPRESENTATION(#12939,#12813);
#12730=PROPERTY_DEFINITION_REPRESENTATION(#12940,#12814);
#12731=PROPERTY_DEFINITION_REPRESENTATION(#12941,#12815);
#12732=PROPERTY_DEFINITION_REPRESENTATION(#12942,#12816);
#12733=PROPERTY_DEFINITION_REPRESENTATION(#12943,#12817);
#12734=PROPERTY_DEFINITION_REPRESENTATION(#12944,#12818);
#12735=PROPERTY_DEFINITION_REPRESENTATION(#12945,#12819);
#12736=PROPERTY_DEFINITION_REPRESENTATION(#12946,#12820);
#12737=PROPERTY_DEFINITION_REPRESENTATION(#12947,#12821);
#12738=PROPERTY_DEFINITION_REPRESENTATION(#12948,#12822);
#12739=PROPERTY_DEFINITION_REPRESENTATION(#12949,#12823);
#12740=PROPERTY_DEFINITION_REPRESENTATION(#12950,#12824);
#12741=PROPERTY_DEFINITION_REPRESENTATION(#12951,#12825);
#12742=PROPERTY_DEFINITION_REPRESENTATION(#12952,#12826);
#12743=PROPERTY_DEFINITION_REPRESENTATION(#12953,#12827);
#12744=PROPERTY_DEFINITION_REPRESENTATION(#12954,#12828);
#12745=PROPERTY_DEFINITION_REPRESENTATION(#12955,#12829);
#12746=PROPERTY_DEFINITION_REPRESENTATION(#12956,#12830);
#12747=PROPERTY_DEFINITION_REPRESENTATION(#12957,#12831);
#12748=PROPERTY_DEFINITION_REPRESENTATION(#12958,#12832);
#12749=PROPERTY_DEFINITION_REPRESENTATION(#12959,#12833);
#12750=PROPERTY_DEFINITION_REPRESENTATION(#12960,#12834);
#12751=PROPERTY_DEFINITION_REPRESENTATION(#12961,#12835);
#12752=PROPERTY_DEFINITION_REPRESENTATION(#12962,#12836);
#12753=PROPERTY_DEFINITION_REPRESENTATION(#12963,#12837);
#12754=PROPERTY_DEFINITION_REPRESENTATION(#12964,#12838);
#12755=PROPERTY_DEFINITION_REPRESENTATION(#12965,#12839);
#12756=PROPERTY_DEFINITION_REPRESENTATION(#12966,#12840);
#12757=PROPERTY_DEFINITION_REPRESENTATION(#12967,#12841);
#12758=PROPERTY_DEFINITION_REPRESENTATION(#12968,#12842);
#12759=PROPERTY_DEFINITION_REPRESENTATION(#12969,#12843);
#12760=PROPERTY_DEFINITION_REPRESENTATION(#12970,#12844);
#12761=PROPERTY_DEFINITION_REPRESENTATION(#12971,#12845);
#12762=PROPERTY_DEFINITION_REPRESENTATION(#12972,#12846);
#12763=PROPERTY_DEFINITION_REPRESENTATION(#12973,#12847);
#12764=PROPERTY_DEFINITION_REPRESENTATION(#12974,#12848);
#12765=PROPERTY_DEFINITION_REPRESENTATION(#12975,#12849);
#12766=PROPERTY_DEFINITION_REPRESENTATION(#12976,#12850);
#12767=PROPERTY_DEFINITION_REPRESENTATION(#12977,#12851);
#12768=PROPERTY_DEFINITION_REPRESENTATION(#12978,#12852);
#12769=PROPERTY_DEFINITION_REPRESENTATION(#12979,#12853);
#12770=PROPERTY_DEFINITION_REPRESENTATION(#12980,#12854);
#12771=PROPERTY_DEFINITION_REPRESENTATION(#12981,#12855);
#12772=PROPERTY_DEFINITION_REPRESENTATION(#12982,#12856);
#12773=PROPERTY_DEFINITION_REPRESENTATION(#12983,#12857);
#12774=PROPERTY_DEFINITION_REPRESENTATION(#12984,#12858);
#12775=PROPERTY_DEFINITION_REPRESENTATION(#12985,#12859);
#12776=PROPERTY_DEFINITION_REPRESENTATION(#12986,#12860);
#12777=PROPERTY_DEFINITION_REPRESENTATION(#12987,#12861);
#12778=PROPERTY_DEFINITION_REPRESENTATION(#12988,#12862);
#12779=PROPERTY_DEFINITION_REPRESENTATION(#12989,#12863);
#12780=PROPERTY_DEFINITION_REPRESENTATION(#12990,#12864);
#12781=PROPERTY_DEFINITION_REPRESENTATION(#12991,#12865);
#12782=PROPERTY_DEFINITION_REPRESENTATION(#12992,#12866);
#12783=PROPERTY_DEFINITION_REPRESENTATION(#12993,#12867);
#12784=PROPERTY_DEFINITION_REPRESENTATION(#12994,#12868);
#12785=PROPERTY_DEFINITION_REPRESENTATION(#12995,#12869);
#12786=PROPERTY_DEFINITION_REPRESENTATION(#12996,#12870);
#12787=PROPERTY_DEFINITION_REPRESENTATION(#12997,#12871);
#12788=PROPERTY_DEFINITION_REPRESENTATION(#12998,#12872);
#12789=REPRESENTATION('material name',(#12873),#32705);
#12790=REPRESENTATION('density',(#12663),#32705);
#12791=REPRESENTATION('material name',(#12874),#32706);
#12792=REPRESENTATION('density',(#12664),#32706);
#12793=REPRESENTATION('material name',(#12875),#32707);
#12794=REPRESENTATION('density',(#12665),#32707);
#12795=REPRESENTATION('material name',(#12876),#32708);
#12796=REPRESENTATION('density',(#12666),#32708);
#12797=REPRESENTATION('material name',(#12877),#32709);
#12798=REPRESENTATION('density',(#12667),#32709);
#12799=REPRESENTATION('material name',(#12878),#32710);
#12800=REPRESENTATION('density',(#12668),#32710);
#12801=REPRESENTATION('material name',(#12879),#32711);
#12802=REPRESENTATION('density',(#12669),#32711);
#12803=REPRESENTATION('material name',(#12880),#32712);
#12804=REPRESENTATION('density',(#12670),#32712);
#12805=REPRESENTATION('material name',(#12881),#32713);
#12806=REPRESENTATION('density',(#12671),#32713);
#12807=REPRESENTATION('material name',(#12882),#32714);
#12808=REPRESENTATION('density',(#12672),#32714);
#12809=REPRESENTATION('material name',(#12883),#32715);
#12810=REPRESENTATION('density',(#12673),#32715);
#12811=REPRESENTATION('material name',(#12884),#32716);
#12812=REPRESENTATION('density',(#12674),#32716);
#12813=REPRESENTATION('material name',(#12885),#32717);
#12814=REPRESENTATION('density',(#12675),#32717);
#12815=REPRESENTATION('material name',(#12886),#32718);
#12816=REPRESENTATION('density',(#12676),#32718);
#12817=REPRESENTATION('material name',(#12887),#32719);
#12818=REPRESENTATION('density',(#12677),#32719);
#12819=REPRESENTATION('material name',(#12888),#32720);
#12820=REPRESENTATION('density',(#12678),#32720);
#12821=REPRESENTATION('material name',(#12889),#32722);
#12822=REPRESENTATION('density',(#12679),#32722);
#12823=REPRESENTATION('material name',(#12890),#32723);
#12824=REPRESENTATION('density',(#12680),#32723);
#12825=REPRESENTATION('material name',(#12891),#32724);
#12826=REPRESENTATION('density',(#12681),#32724);
#12827=REPRESENTATION('material name',(#12892),#32725);
#12828=REPRESENTATION('density',(#12682),#32725);
#12829=REPRESENTATION('material name',(#12893),#32726);
#12830=REPRESENTATION('density',(#12683),#32726);
#12831=REPRESENTATION('material name',(#12894),#32727);
#12832=REPRESENTATION('density',(#12684),#32727);
#12833=REPRESENTATION('material name',(#12895),#32729);
#12834=REPRESENTATION('density',(#12685),#32729);
#12835=REPRESENTATION('material name',(#12896),#32730);
#12836=REPRESENTATION('density',(#12686),#32730);
#12837=REPRESENTATION('material name',(#12897),#32731);
#12838=REPRESENTATION('density',(#12687),#32731);
#12839=REPRESENTATION('material name',(#12898),#32732);
#12840=REPRESENTATION('density',(#12688),#32732);
#12841=REPRESENTATION('material name',(#12899),#32734);
#12842=REPRESENTATION('density',(#12689),#32734);
#12843=REPRESENTATION('material name',(#12900),#32735);
#12844=REPRESENTATION('density',(#12690),#32735);
#12845=REPRESENTATION('material name',(#12901),#32736);
#12846=REPRESENTATION('density',(#12691),#32736);
#12847=REPRESENTATION('material name',(#12902),#32737);
#12848=REPRESENTATION('density',(#12692),#32737);
#12849=REPRESENTATION('material name',(#12903),#32738);
#12850=REPRESENTATION('density',(#12693),#32738);
#12851=REPRESENTATION('material name',(#12904),#32739);
#12852=REPRESENTATION('density',(#12694),#32739);
#12853=REPRESENTATION('material name',(#12905),#32740);
#12854=REPRESENTATION('density',(#12695),#32740);
#12855=REPRESENTATION('material name',(#12906),#32741);
#12856=REPRESENTATION('density',(#12696),#32741);
#12857=REPRESENTATION('material name',(#12907),#32742);
#12858=REPRESENTATION('density',(#12697),#32742);
#12859=REPRESENTATION('material name',(#12908),#32743);
#12860=REPRESENTATION('density',(#12698),#32743);
#12861=REPRESENTATION('material name',(#12909),#32744);
#12862=REPRESENTATION('density',(#12699),#32744);
#12863=REPRESENTATION('material name',(#12910),#32745);
#12864=REPRESENTATION('density',(#12700),#32745);
#12865=REPRESENTATION('material name',(#12911),#32746);
#12866=REPRESENTATION('density',(#12701),#32746);
#12867=REPRESENTATION('material name',(#12912),#32747);
#12868=REPRESENTATION('density',(#12702),#32747);
#12869=REPRESENTATION('material name',(#12913),#32748);
#12870=REPRESENTATION('density',(#12703),#32748);
#12871=REPRESENTATION('material name',(#12914),#32750);
#12872=REPRESENTATION('density',(#12704),#32750);
#12873=DESCRIPTIVE_REPRESENTATION_ITEM('Steel','Steel');
#12874=DESCRIPTIVE_REPRESENTATION_ITEM('Steel','Steel');
#12875=DESCRIPTIVE_REPRESENTATION_ITEM('Steel','Steel');
#12876=DESCRIPTIVE_REPRESENTATION_ITEM('Steel','Steel');
#12877=DESCRIPTIVE_REPRESENTATION_ITEM('Steel','Steel');
#12878=DESCRIPTIVE_REPRESENTATION_ITEM('Steel','Steel');
#12879=DESCRIPTIVE_REPRESENTATION_ITEM('Steel','Steel');
#12880=DESCRIPTIVE_REPRESENTATION_ITEM('Steel','Steel');
#12881=DESCRIPTIVE_REPRESENTATION_ITEM('Steel','Steel');
#12882=DESCRIPTIVE_REPRESENTATION_ITEM('Steel','Steel');
#12883=DESCRIPTIVE_REPRESENTATION_ITEM('Steel','Steel');
#12884=DESCRIPTIVE_REPRESENTATION_ITEM('Steel','Steel');
#12885=DESCRIPTIVE_REPRESENTATION_ITEM('Steel','Steel');
#12886=DESCRIPTIVE_REPRESENTATION_ITEM('Steel','Steel');
#12887=DESCRIPTIVE_REPRESENTATION_ITEM('Steel','Steel');
#12888=DESCRIPTIVE_REPRESENTATION_ITEM('Steel','Steel');
#12889=DESCRIPTIVE_REPRESENTATION_ITEM('Steel','Steel');
#12890=DESCRIPTIVE_REPRESENTATION_ITEM('Steel','Steel');
#12891=DESCRIPTIVE_REPRESENTATION_ITEM('Steel','Steel');
#12892=DESCRIPTIVE_REPRESENTATION_ITEM('Steel','Steel');
#12893=DESCRIPTIVE_REPRESENTATION_ITEM('Steel','Steel');
#12894=DESCRIPTIVE_REPRESENTATION_ITEM('Steel','Steel');
#12895=DESCRIPTIVE_REPRESENTATION_ITEM('Steel','Steel');
#12896=DESCRIPTIVE_REPRESENTATION_ITEM('Steel','Steel');
#12897=DESCRIPTIVE_REPRESENTATION_ITEM('Steel','Steel');
#12898=DESCRIPTIVE_REPRESENTATION_ITEM('Steel','Steel');
#12899=DESCRIPTIVE_REPRESENTATION_ITEM('Steel','Steel');
#12900=DESCRIPTIVE_REPRESENTATION_ITEM('Steel','Steel');
#12901=DESCRIPTIVE_REPRESENTATION_ITEM('Steel','Steel');
#12902=DESCRIPTIVE_REPRESENTATION_ITEM('Steel','Steel');
#12903=DESCRIPTIVE_REPRESENTATION_ITEM('Steel','Steel');
#12904=DESCRIPTIVE_REPRESENTATION_ITEM('Steel','Steel');
#12905=DESCRIPTIVE_REPRESENTATION_ITEM('Steel','Steel');
#12906=DESCRIPTIVE_REPRESENTATION_ITEM('Steel','Steel');
#12907=DESCRIPTIVE_REPRESENTATION_ITEM('Steel','Steel');
#12908=DESCRIPTIVE_REPRESENTATION_ITEM('Steel','Steel');
#12909=DESCRIPTIVE_REPRESENTATION_ITEM('Steel','Steel');
#12910=DESCRIPTIVE_REPRESENTATION_ITEM('Steel','Steel');
#12911=DESCRIPTIVE_REPRESENTATION_ITEM('Steel','Steel');
#12912=DESCRIPTIVE_REPRESENTATION_ITEM('Steel','Steel');
#12913=DESCRIPTIVE_REPRESENTATION_ITEM('Steel','Steel');
#12914=DESCRIPTIVE_REPRESENTATION_ITEM('Steel','Steel');
#12915=PROPERTY_DEFINITION('material property','material name',#32980);
#12916=PROPERTY_DEFINITION('material property','density of part',#32980);
#12917=PROPERTY_DEFINITION('material property','material name',#32981);
#12918=PROPERTY_DEFINITION('material property','density of part',#32981);
#12919=PROPERTY_DEFINITION('material property','material name',#32982);
#12920=PROPERTY_DEFINITION('material property','density of part',#32982);
#12921=PROPERTY_DEFINITION('material property','material name',#32983);
#12922=PROPERTY_DEFINITION('material property','density of part',#32983);
#12923=PROPERTY_DEFINITION('material property','material name',#32984);
#12924=PROPERTY_DEFINITION('material property','density of part',#32984);
#12925=PROPERTY_DEFINITION('material property','material name',#32985);
#12926=PROPERTY_DEFINITION('material property','density of part',#32985);
#12927=PROPERTY_DEFINITION('material property','material name',#32986);
#12928=PROPERTY_DEFINITION('material property','density of part',#32986);
#12929=PROPERTY_DEFINITION('material property','material name',#32987);
#12930=PROPERTY_DEFINITION('material property','density of part',#32987);
#12931=PROPERTY_DEFINITION('material property','material name',#32988);
#12932=PROPERTY_DEFINITION('material property','density of part',#32988);
#12933=PROPERTY_DEFINITION('material property','material name',#32989);
#12934=PROPERTY_DEFINITION('material property','density of part',#32989);
#12935=PROPERTY_DEFINITION('material property','material name',#32990);
#12936=PROPERTY_DEFINITION('material property','density of part',#32990);
#12937=PROPERTY_DEFINITION('material property','material name',#32991);
#12938=PROPERTY_DEFINITION('material property','density of part',#32991);
#12939=PROPERTY_DEFINITION('material property','material name',#32992);
#12940=PROPERTY_DEFINITION('material property','density of part',#32992);
#12941=PROPERTY_DEFINITION('material property','material name',#32993);
#12942=PROPERTY_DEFINITION('material property','density of part',#32993);
#12943=PROPERTY_DEFINITION('material property','material name',#32994);
#12944=PROPERTY_DEFINITION('material property','density of part',#32994);
#12945=PROPERTY_DEFINITION('material property','material name',#32995);
#12946=PROPERTY_DEFINITION('material property','density of part',#32995);
#12947=PROPERTY_DEFINITION('material property','material name',#32997);
#12948=PROPERTY_DEFINITION('material property','density of part',#32997);
#12949=PROPERTY_DEFINITION('material property','material name',#32998);
#12950=PROPERTY_DEFINITION('material property','density of part',#32998);
#12951=PROPERTY_DEFINITION('material property','material name',#32999);
#12952=PROPERTY_DEFINITION('material property','density of part',#32999);
#12953=PROPERTY_DEFINITION('material property','material name',#33000);
#12954=PROPERTY_DEFINITION('material property','density of part',#33000);
#12955=PROPERTY_DEFINITION('material property','material name',#33001);
#12956=PROPERTY_DEFINITION('material property','density of part',#33001);
#12957=PROPERTY_DEFINITION('material property','material name',#33002);
#12958=PROPERTY_DEFINITION('material property','density of part',#33002);
#12959=PROPERTY_DEFINITION('material property','material name',#33004);
#12960=PROPERTY_DEFINITION('material property','density of part',#33004);
#12961=PROPERTY_DEFINITION('material property','material name',#33005);
#12962=PROPERTY_DEFINITION('material property','density of part',#33005);
#12963=PROPERTY_DEFINITION('material property','material name',#33006);
#12964=PROPERTY_DEFINITION('material property','density of part',#33006);
#12965=PROPERTY_DEFINITION('material property','material name',#33007);
#12966=PROPERTY_DEFINITION('material property','density of part',#33007);
#12967=PROPERTY_DEFINITION('material property','material name',#33009);
#12968=PROPERTY_DEFINITION('material property','density of part',#33009);
#12969=PROPERTY_DEFINITION('material property','material name',#33010);
#12970=PROPERTY_DEFINITION('material property','density of part',#33010);
#12971=PROPERTY_DEFINITION('material property','material name',#33011);
#12972=PROPERTY_DEFINITION('material property','density of part',#33011);
#12973=PROPERTY_DEFINITION('material property','material name',#33012);
#12974=PROPERTY_DEFINITION('material property','density of part',#33012);
#12975=PROPERTY_DEFINITION('material property','material name',#33013);
#12976=PROPERTY_DEFINITION('material property','density of part',#33013);
#12977=PROPERTY_DEFINITION('material property','material name',#33014);
#12978=PROPERTY_DEFINITION('material property','density of part',#33014);
#12979=PROPERTY_DEFINITION('material property','material name',#33015);
#12980=PROPERTY_DEFINITION('material property','density of part',#33015);
#12981=PROPERTY_DEFINITION('material property','material name',#33016);
#12982=PROPERTY_DEFINITION('material property','density of part',#33016);
#12983=PROPERTY_DEFINITION('material property','material name',#33017);
#12984=PROPERTY_DEFINITION('material property','density of part',#33017);
#12985=PROPERTY_DEFINITION('material property','material name',#33018);
#12986=PROPERTY_DEFINITION('material property','density of part',#33018);
#12987=PROPERTY_DEFINITION('material property','material name',#33019);
#12988=PROPERTY_DEFINITION('material property','density of part',#33019);
#12989=PROPERTY_DEFINITION('material property','material name',#33020);
#12990=PROPERTY_DEFINITION('material property','density of part',#33020);
#12991=PROPERTY_DEFINITION('material property','material name',#33021);
#12992=PROPERTY_DEFINITION('material property','density of part',#33021);
#12993=PROPERTY_DEFINITION('material property','material name',#33022);
#12994=PROPERTY_DEFINITION('material property','density of part',#33022);
#12995=PROPERTY_DEFINITION('material property','material name',#33023);
#12996=PROPERTY_DEFINITION('material property','density of part',#33023);
#12997=PROPERTY_DEFINITION('material property','material name',#33025);
#12998=PROPERTY_DEFINITION('material property','density of part',#33025);
#12999=AXIS2_PLACEMENT_3D('',#17638,#14155,#14156);
#13000=AXIS2_PLACEMENT_3D('',#17639,#14157,#14158);
#13001=AXIS2_PLACEMENT_3D('',#17640,#14159,#14160);
#13002=AXIS2_PLACEMENT_3D('',#17641,#14161,#14162);
#13003=AXIS2_PLACEMENT_3D('',#17643,#14163,#14164);
#13004=AXIS2_PLACEMENT_3D('',#17646,#14166,#14167);
#13005=AXIS2_PLACEMENT_3D('',#17647,#14168,#14169);
#13006=AXIS2_PLACEMENT_3D('',#17649,#14170,#14171);
#13007=AXIS2_PLACEMENT_3D('',#17652,#14173,#14174);
#13008=AXIS2_PLACEMENT_3D('',#17653,#14175,#14176);
#13009=AXIS2_PLACEMENT_3D('',#17655,#14177,#14178);
#13010=AXIS2_PLACEMENT_3D('',#17658,#14180,#14181);
#13011=AXIS2_PLACEMENT_3D('',#17659,#14182,#14183);
#13012=AXIS2_PLACEMENT_3D('',#17661,#14184,#14185);
#13013=AXIS2_PLACEMENT_3D('',#17664,#14187,#14188);
#13014=AXIS2_PLACEMENT_3D('',#17665,#14189,#14190);
#13015=AXIS2_PLACEMENT_3D('',#17667,#14191,#14192);
#13016=AXIS2_PLACEMENT_3D('',#17670,#14194,#14195);
#13017=AXIS2_PLACEMENT_3D('',#17671,#14196,#14197);
#13018=AXIS2_PLACEMENT_3D('',#17673,#14198,#14199);
#13019=AXIS2_PLACEMENT_3D('',#17676,#14201,#14202);
#13020=AXIS2_PLACEMENT_3D('',#17677,#14203,#14204);
#13021=AXIS2_PLACEMENT_3D('',#17679,#14205,#14206);
#13022=AXIS2_PLACEMENT_3D('',#17682,#14208,#14209);
#13023=AXIS2_PLACEMENT_3D('',#17683,#14210,#14211);
#13024=AXIS2_PLACEMENT_3D('',#17685,#14212,#14213);
#13025=AXIS2_PLACEMENT_3D('',#17688,#14215,#14216);
#13026=AXIS2_PLACEMENT_3D('',#17689,#14217,#14218);
#13027=AXIS2_PLACEMENT_3D('',#17691,#14219,#14220);
#13028=AXIS2_PLACEMENT_3D('',#17694,#14222,#14223);
#13029=AXIS2_PLACEMENT_3D('',#17695,#14224,#14225);
#13030=AXIS2_PLACEMENT_3D('',#17697,#14226,#14227);
#13031=AXIS2_PLACEMENT_3D('',#17700,#14229,#14230);
#13032=AXIS2_PLACEMENT_3D('',#17701,#14231,#14232);
#13033=AXIS2_PLACEMENT_3D('',#17710,#14237,#14238);
#13034=AXIS2_PLACEMENT_3D('',#17716,#14242,#14243);
#13035=AXIS2_PLACEMENT_3D('',#17722,#14247,#14248);
#13036=AXIS2_PLACEMENT_3D('',#17725,#14251,#14252);
#13037=AXIS2_PLACEMENT_3D('',#17726,#14253,#14254);
#13038=AXIS2_PLACEMENT_3D('',#17727,#14255,#14256);
#13039=AXIS2_PLACEMENT_3D('',#17728,#14257,#14258);
#13040=AXIS2_PLACEMENT_3D('',#17737,#14263,#14264);
#13041=AXIS2_PLACEMENT_3D('',#17743,#14268,#14269);
#13042=AXIS2_PLACEMENT_3D('',#17749,#14273,#14274);
#13043=AXIS2_PLACEMENT_3D('',#17752,#14277,#14278);
#13044=AXIS2_PLACEMENT_3D('',#17753,#14279,#14280);
#13045=AXIS2_PLACEMENT_3D('',#17754,#14281,#14282);
#13046=AXIS2_PLACEMENT_3D('',#17755,#14283,#14284);
#13047=AXIS2_PLACEMENT_3D('',#17764,#14289,#14290);
#13048=AXIS2_PLACEMENT_3D('',#17770,#14294,#14295);
#13049=AXIS2_PLACEMENT_3D('',#17776,#14299,#14300);
#13050=AXIS2_PLACEMENT_3D('',#17779,#14303,#14304);
#13051=AXIS2_PLACEMENT_3D('',#17780,#14305,#14306);
#13052=AXIS2_PLACEMENT_3D('',#17781,#14307,#14308);
#13053=AXIS2_PLACEMENT_3D('',#17782,#14309,#14310);
#13054=AXIS2_PLACEMENT_3D('',#17784,#14311,#14312);
#13055=AXIS2_PLACEMENT_3D('',#17787,#14314,#14315);
#13056=AXIS2_PLACEMENT_3D('',#17788,#14316,#14317);
#13057=AXIS2_PLACEMENT_3D('',#17789,#14318,#14319);
#13058=AXIS2_PLACEMENT_3D('',#17791,#14320,#14321);
#13059=AXIS2_PLACEMENT_3D('',#17794,#14323,#14324);
#13060=AXIS2_PLACEMENT_3D('',#17795,#14325,#14326);
#13061=AXIS2_PLACEMENT_3D('',#17796,#14327,#14328);
#13062=AXIS2_PLACEMENT_3D('',#17805,#14333,#14334);
#13063=AXIS2_PLACEMENT_3D('',#17814,#14339,#14340);
#13064=AXIS2_PLACEMENT_3D('',#17816,#14341,#14342);
#13065=AXIS2_PLACEMENT_3D('',#17823,#14346,#14347);
#13066=AXIS2_PLACEMENT_3D('',#17824,#14348,#14349);
#13067=AXIS2_PLACEMENT_3D('',#17825,#14350,#14351);
#13068=AXIS2_PLACEMENT_3D('',#17826,#14352,#14353);
#13069=AXIS2_PLACEMENT_3D('',#17827,#14354,#14355);
#13070=AXIS2_PLACEMENT_3D('',#17830,#14357,#14358);
#13071=AXIS2_PLACEMENT_3D('',#17831,#14359,#14360);
#13072=AXIS2_PLACEMENT_3D('',#17833,#14361,#14362);
#13073=AXIS2_PLACEMENT_3D('',#17835,#14364,#14365);
#13074=AXIS2_PLACEMENT_3D('',#17841,#14369,#14370);
#13075=AXIS2_PLACEMENT_3D('',#17843,#14372,#14373);
#13076=AXIS2_PLACEMENT_3D('',#17845,#14375,#14376);
#13077=AXIS2_PLACEMENT_3D('',#17847,#14377,#14378);
#13078=AXIS2_PLACEMENT_3D('',#17850,#14380,#14381);
#13079=AXIS2_PLACEMENT_3D('',#17851,#14382,#14383);
#13080=AXIS2_PLACEMENT_3D('',#17852,#14384,#14385);
#13081=AXIS2_PLACEMENT_3D('',#17854,#14386,#14387);
#13082=AXIS2_PLACEMENT_3D('',#17857,#14389,#14390);
#13083=AXIS2_PLACEMENT_3D('',#17858,#14391,#14392);
#13084=AXIS2_PLACEMENT_3D('',#17859,#14393,#14394);
#13085=AXIS2_PLACEMENT_3D('',#17868,#14399,#14400);
#13086=AXIS2_PLACEMENT_3D('',#17877,#14405,#14406);
#13087=AXIS2_PLACEMENT_3D('',#17879,#14407,#14408);
#13088=AXIS2_PLACEMENT_3D('',#17886,#14412,#14413);
#13089=AXIS2_PLACEMENT_3D('',#17887,#14414,#14415);
#13090=AXIS2_PLACEMENT_3D('',#17888,#14416,#14417);
#13091=AXIS2_PLACEMENT_3D('',#17889,#14418,#14419);
#13092=AXIS2_PLACEMENT_3D('',#17890,#14420,#14421);
#13093=AXIS2_PLACEMENT_3D('',#17893,#14423,#14424);
#13094=AXIS2_PLACEMENT_3D('',#17894,#14425,#14426);
#13095=AXIS2_PLACEMENT_3D('',#17896,#14427,#14428);
#13096=AXIS2_PLACEMENT_3D('',#17898,#14430,#14431);
#13097=AXIS2_PLACEMENT_3D('',#17904,#14435,#14436);
#13098=AXIS2_PLACEMENT_3D('',#17906,#14438,#14439);
#13099=AXIS2_PLACEMENT_3D('',#17908,#14441,#14442);
#13100=AXIS2_PLACEMENT_3D('',#17910,#14443,#14444);
#13101=AXIS2_PLACEMENT_3D('',#17913,#14446,#14447);
#13102=AXIS2_PLACEMENT_3D('',#17914,#14448,#14449);
#13103=AXIS2_PLACEMENT_3D('',#17916,#14450,#14451);
#13104=AXIS2_PLACEMENT_3D('',#17919,#14453,#14454);
#13105=AXIS2_PLACEMENT_3D('',#17920,#14455,#14456);
#13106=AXIS2_PLACEMENT_3D('',#17922,#14457,#14458);
#13107=AXIS2_PLACEMENT_3D('',#17925,#14460,#14461);
#13108=AXIS2_PLACEMENT_3D('',#17926,#14462,#14463);
#13109=AXIS2_PLACEMENT_3D('',#17928,#14464,#14465);
#13110=AXIS2_PLACEMENT_3D('',#17931,#14467,#14468);
#13111=AXIS2_PLACEMENT_3D('',#17932,#14469,#14470);
#13112=AXIS2_PLACEMENT_3D('',#17949,#14479,#14480);
#13113=AXIS2_PLACEMENT_3D('',#17955,#14484,#14485);
#13114=AXIS2_PLACEMENT_3D('',#17959,#14488,#14489);
#13115=AXIS2_PLACEMENT_3D('',#17963,#14492,#14493);
#13116=AXIS2_PLACEMENT_3D('',#17965,#14495,#14496);
#13117=AXIS2_PLACEMENT_3D('',#17971,#14500,#14501);
#13118=AXIS2_PLACEMENT_3D('',#17975,#14504,#14505);
#13119=AXIS2_PLACEMENT_3D('',#17979,#14508,#14509);
#13120=AXIS2_PLACEMENT_3D('',#17981,#14511,#14512);
#13121=AXIS2_PLACEMENT_3D('',#17982,#14513,#14514);
#13122=AXIS2_PLACEMENT_3D('',#17983,#14515,#14516);
#13123=AXIS2_PLACEMENT_3D('',#17984,#14517,#14518);
#13124=AXIS2_PLACEMENT_3D('',#17993,#14523,#14524);
#13125=AXIS2_PLACEMENT_3D('',#18002,#14529,#14530);
#13126=AXIS2_PLACEMENT_3D('',#18012,#14536,#14537);
#13127=AXIS2_PLACEMENT_3D('',#18022,#14543,#14544);
#13128=AXIS2_PLACEMENT_3D('',#18023,#14545,#14546);
#13129=AXIS2_PLACEMENT_3D('',#18024,#14547,#14548);
#13130=AXIS2_PLACEMENT_3D('',#18025,#14549,#14550);
#13131=AXIS2_PLACEMENT_3D('',#18026,#14551,#14552);
#13132=AXIS2_PLACEMENT_3D('',#18027,#14553,#14554);
#13133=AXIS2_PLACEMENT_3D('',#18028,#14555,#14556);
#13134=AXIS2_PLACEMENT_3D('',#18029,#14557,#14558);
#13135=AXIS2_PLACEMENT_3D('',#18030,#14559,#14560);
#13136=AXIS2_PLACEMENT_3D('',#18031,#14561,#14562);
#13137=AXIS2_PLACEMENT_3D('',#18032,#14563,#14564);
#13138=AXIS2_PLACEMENT_3D('',#18033,#14565,#14566);
#13139=AXIS2_PLACEMENT_3D('',#18034,#14567,#14568);
#13140=AXIS2_PLACEMENT_3D('',#18035,#14569,#14570);
#13141=AXIS2_PLACEMENT_3D('',#18037,#14571,#14572);
#13142=AXIS2_PLACEMENT_3D('',#18040,#14574,#14575);
#13143=AXIS2_PLACEMENT_3D('',#18041,#14576,#14577);
#13144=AXIS2_PLACEMENT_3D('',#18043,#14578,#14579);
#13145=AXIS2_PLACEMENT_3D('',#18046,#14581,#14582);
#13146=AXIS2_PLACEMENT_3D('',#18047,#14583,#14584);
#13147=AXIS2_PLACEMENT_3D('',#18056,#14589,#14590);
#13148=AXIS2_PLACEMENT_3D('',#18065,#14595,#14596);
#13149=AXIS2_PLACEMENT_3D('',#18071,#14600,#14601);
#13150=AXIS2_PLACEMENT_3D('',#18077,#14605,#14606);
#13151=AXIS2_PLACEMENT_3D('',#18083,#14610,#14611);
#13152=AXIS2_PLACEMENT_3D('',#18089,#14615,#14616);
#13153=AXIS2_PLACEMENT_3D('',#18090,#14617,#14618);
#13154=AXIS2_PLACEMENT_3D('',#18096,#14622,#14623);
#13155=AXIS2_PLACEMENT_3D('',#18097,#14624,#14625);
#13156=AXIS2_PLACEMENT_3D('',#18098,#14626,#14627);
#13157=AXIS2_PLACEMENT_3D('',#18102,#14630,#14631);
#13158=AXIS2_PLACEMENT_3D('',#18106,#14634,#14635);
#13159=AXIS2_PLACEMENT_3D('',#18108,#14637,#14638);
#13160=AXIS2_PLACEMENT_3D('',#18109,#14639,#14640);
#13161=AXIS2_PLACEMENT_3D('',#18110,#14641,#14642);
#13162=AXIS2_PLACEMENT_3D('',#18119,#14647,#14648);
#13163=AXIS2_PLACEMENT_3D('',#18128,#14653,#14654);
#13164=AXIS2_PLACEMENT_3D('',#18138,#14660,#14661);
#13165=AXIS2_PLACEMENT_3D('',#18148,#14667,#14668);
#13166=AXIS2_PLACEMENT_3D('',#18149,#14669,#14670);
#13167=AXIS2_PLACEMENT_3D('',#18150,#14671,#14672);
#13168=AXIS2_PLACEMENT_3D('',#18151,#14673,#14674);
#13169=AXIS2_PLACEMENT_3D('',#18152,#14675,#14676);
#13170=AXIS2_PLACEMENT_3D('',#18153,#14677,#14678);
#13171=AXIS2_PLACEMENT_3D('',#18154,#14679,#14680);
#13172=AXIS2_PLACEMENT_3D('',#18155,#14681,#14682);
#13173=AXIS2_PLACEMENT_3D('',#18156,#14683,#14684);
#13174=AXIS2_PLACEMENT_3D('',#18157,#14685,#14686);
#13175=AXIS2_PLACEMENT_3D('',#18158,#14687,#14688);
#13176=AXIS2_PLACEMENT_3D('',#18159,#14689,#14690);
#13177=AXIS2_PLACEMENT_3D('',#18160,#14691,#14692);
#13178=AXIS2_PLACEMENT_3D('',#18161,#14693,#14694);
#13179=AXIS2_PLACEMENT_3D('',#18163,#14695,#14696);
#13180=AXIS2_PLACEMENT_3D('',#18166,#14698,#14699);
#13181=AXIS2_PLACEMENT_3D('',#18167,#14700,#14701);
#13182=AXIS2_PLACEMENT_3D('',#18169,#14702,#14703);
#13183=AXIS2_PLACEMENT_3D('',#18172,#14705,#14706);
#13184=AXIS2_PLACEMENT_3D('',#18173,#14707,#14708);
#13185=AXIS2_PLACEMENT_3D('',#18182,#14713,#14714);
#13186=AXIS2_PLACEMENT_3D('',#18191,#14719,#14720);
#13187=AXIS2_PLACEMENT_3D('',#18197,#14724,#14725);
#13188=AXIS2_PLACEMENT_3D('',#18203,#14729,#14730);
#13189=AXIS2_PLACEMENT_3D('',#18209,#14734,#14735);
#13190=AXIS2_PLACEMENT_3D('',#18215,#14739,#14740);
#13191=AXIS2_PLACEMENT_3D('',#18216,#14741,#14742);
#13192=AXIS2_PLACEMENT_3D('',#18222,#14746,#14747);
#13193=AXIS2_PLACEMENT_3D('',#18223,#14748,#14749);
#13194=AXIS2_PLACEMENT_3D('',#18224,#14750,#14751);
#13195=AXIS2_PLACEMENT_3D('',#18228,#14754,#14755);
#13196=AXIS2_PLACEMENT_3D('',#18232,#14758,#14759);
#13197=AXIS2_PLACEMENT_3D('',#18234,#14761,#14762);
#13198=AXIS2_PLACEMENT_3D('',#18235,#14763,#14764);
#13199=AXIS2_PLACEMENT_3D('',#18236,#14765,#14766);
#13200=AXIS2_PLACEMENT_3D('',#18238,#14767,#14768);
#13201=AXIS2_PLACEMENT_3D('',#18241,#14770,#14771);
#13202=AXIS2_PLACEMENT_3D('',#18242,#14772,#14773);
#13203=AXIS2_PLACEMENT_3D('',#18244,#14774,#14775);
#13204=AXIS2_PLACEMENT_3D('',#18245,#14776,#14777);
#13205=AXIS2_PLACEMENT_3D('',#18247,#14778,#14779);
#13206=AXIS2_PLACEMENT_3D('',#18250,#14781,#14782);
#13207=AXIS2_PLACEMENT_3D('',#18251,#14783,#14784);
#13208=AXIS2_PLACEMENT_3D('',#18253,#14785,#14786);
#13209=AXIS2_PLACEMENT_3D('',#18254,#14787,#14788);
#13210=AXIS2_PLACEMENT_3D('',#18256,#14789,#14790);
#13211=AXIS2_PLACEMENT_3D('',#18258,#14792,#14793);
#13212=AXIS2_PLACEMENT_3D('',#18260,#14794,#14795);
#13213=AXIS2_PLACEMENT_3D('',#18262,#14797,#14798);
#13214=AXIS2_PLACEMENT_3D('',#18264,#14799,#14800);
#13215=AXIS2_PLACEMENT_3D('',#18267,#14802,#14803);
#13216=AXIS2_PLACEMENT_3D('',#18268,#14804,#14805);
#13217=AXIS2_PLACEMENT_3D('',#18269,#14806,#14807);
#13218=AXIS2_PLACEMENT_3D('',#18270,#14808,#14809);
#13219=AXIS2_PLACEMENT_3D('',#18271,#14810,#14811);
#13220=AXIS2_PLACEMENT_3D('',#18274,#14812,#14813);
#13221=AXIS2_PLACEMENT_3D('',#18278,#14815,#14816);
#13222=AXIS2_PLACEMENT_3D('',#18280,#14818,#14819);
#13223=AXIS2_PLACEMENT_3D('',#18289,#14824,#14825);
#13224=AXIS2_PLACEMENT_3D('',#18291,#14826,#14827);
#13225=AXIS2_PLACEMENT_3D('',#18292,#14828,#14829);
#13226=AXIS2_PLACEMENT_3D('',#18296,#14832,#14833);
#13227=AXIS2_PLACEMENT_3D('',#18298,#14834,#14835);
#13228=AXIS2_PLACEMENT_3D('',#18301,#14837,#14838);
#13229=AXIS2_PLACEMENT_3D('',#18302,#14839,#14840);
#13230=AXIS2_PLACEMENT_3D('',#18304,#14841,#14842);
#13231=AXIS2_PLACEMENT_3D('',#18307,#14844,#14845);
#13232=AXIS2_PLACEMENT_3D('',#18308,#14846,#14847);
#13233=AXIS2_PLACEMENT_3D('',#18310,#14848,#14849);
#13234=AXIS2_PLACEMENT_3D('',#18313,#14851,#14852);
#13235=AXIS2_PLACEMENT_3D('',#18314,#14853,#14854);
#13236=AXIS2_PLACEMENT_3D('',#18316,#14855,#14856);
#13237=AXIS2_PLACEMENT_3D('',#18319,#14858,#14859);
#13238=AXIS2_PLACEMENT_3D('',#18320,#14860,#14861);
#13239=AXIS2_PLACEMENT_3D('',#18323,#14863,#14864);
#13240=AXIS2_PLACEMENT_3D('',#18324,#14865,#14866);
#13241=AXIS2_PLACEMENT_3D('',#18327,#14868,#14869);
#13242=AXIS2_PLACEMENT_3D('',#18328,#14870,#14871);
#13243=AXIS2_PLACEMENT_3D('',#18330,#14872,#14873);
#13244=AXIS2_PLACEMENT_3D('',#18333,#14875,#14876);
#13245=AXIS2_PLACEMENT_3D('',#18334,#14877,#14878);
#13246=AXIS2_PLACEMENT_3D('',#18340,#14882,#14883);
#13247=AXIS2_PLACEMENT_3D('',#18349,#14888,#14889);
#13248=AXIS2_PLACEMENT_3D('',#18352,#14892,#14893);
#13249=AXIS2_PLACEMENT_3D('',#18358,#14897,#14898);
#13250=AXIS2_PLACEMENT_3D('',#18362,#14901,#14902);
#13251=AXIS2_PLACEMENT_3D('',#18366,#14905,#14906);
#13252=AXIS2_PLACEMENT_3D('',#18368,#14908,#14909);
#13253=AXIS2_PLACEMENT_3D('',#18369,#14910,#14911);
#13254=AXIS2_PLACEMENT_3D('',#18370,#14912,#14913);
#13255=AXIS2_PLACEMENT_3D('',#18372,#14914,#14915);
#13256=AXIS2_PLACEMENT_3D('',#18375,#14917,#14918);
#13257=AXIS2_PLACEMENT_3D('',#18376,#14919,#14920);
#13258=AXIS2_PLACEMENT_3D('',#18378,#14921,#14922);
#13259=AXIS2_PLACEMENT_3D('',#18381,#14924,#14925);
#13260=AXIS2_PLACEMENT_3D('',#18382,#14926,#14927);
#13261=AXIS2_PLACEMENT_3D('',#18384,#14928,#14929);
#13262=AXIS2_PLACEMENT_3D('',#18387,#14931,#14932);
#13263=AXIS2_PLACEMENT_3D('',#18388,#14933,#14934);
#13264=AXIS2_PLACEMENT_3D('',#18390,#14935,#14936);
#13265=AXIS2_PLACEMENT_3D('',#18393,#14938,#14939);
#13266=AXIS2_PLACEMENT_3D('',#18394,#14940,#14941);
#13267=AXIS2_PLACEMENT_3D('',#18396,#14942,#14943);
#13268=AXIS2_PLACEMENT_3D('',#18399,#14945,#14946);
#13269=AXIS2_PLACEMENT_3D('',#18400,#14947,#14948);
#13270=AXIS2_PLACEMENT_3D('',#18402,#14949,#14950);
#13271=AXIS2_PLACEMENT_3D('',#18405,#14952,#14953);
#13272=AXIS2_PLACEMENT_3D('',#18406,#14954,#14955);
#13273=AXIS2_PLACEMENT_3D('',#18407,#14956,#14957);
#13274=AXIS2_PLACEMENT_3D('',#18409,#14958,#14959);
#13275=AXIS2_PLACEMENT_3D('',#18412,#14961,#14962);
#13276=AXIS2_PLACEMENT_3D('',#18413,#14963,#14964);
#13277=AXIS2_PLACEMENT_3D('',#18414,#14965,#14966);
#13278=AXIS2_PLACEMENT_3D('',#18415,#14967,#14968);
#13279=AXIS2_PLACEMENT_3D('',#18416,#14969,#14970);
#13280=AXIS2_PLACEMENT_3D('',#18418,#14971,#14972);
#13281=AXIS2_PLACEMENT_3D('',#18421,#14974,#14975);
#13282=AXIS2_PLACEMENT_3D('',#18422,#14976,#14977);
#13283=AXIS2_PLACEMENT_3D('',#18424,#14978,#14979);
#13284=AXIS2_PLACEMENT_3D('',#18427,#14981,#14982);
#13285=AXIS2_PLACEMENT_3D('',#18428,#14983,#14984);
#13286=AXIS2_PLACEMENT_3D('',#18430,#14985,#14986);
#13287=AXIS2_PLACEMENT_3D('',#18433,#14988,#14989);
#13288=AXIS2_PLACEMENT_3D('',#18434,#14990,#14991);
#13289=AXIS2_PLACEMENT_3D('',#18436,#14992,#14993);
#13290=AXIS2_PLACEMENT_3D('',#18439,#14995,#14996);
#13291=AXIS2_PLACEMENT_3D('',#18440,#14997,#14998);
#13292=AXIS2_PLACEMENT_3D('',#18442,#14999,#15000);
#13293=AXIS2_PLACEMENT_3D('',#18445,#15002,#15003);
#13294=AXIS2_PLACEMENT_3D('',#18446,#15004,#15005);
#13295=AXIS2_PLACEMENT_3D('',#18448,#15006,#15007);
#13296=AXIS2_PLACEMENT_3D('',#18451,#15009,#15010);
#13297=AXIS2_PLACEMENT_3D('',#18452,#15011,#15012);
#13298=AXIS2_PLACEMENT_3D('',#18453,#15013,#15014);
#13299=AXIS2_PLACEMENT_3D('',#18455,#15015,#15016);
#13300=AXIS2_PLACEMENT_3D('',#18458,#15018,#15019);
#13301=AXIS2_PLACEMENT_3D('',#18459,#15020,#15021);
#13302=AXIS2_PLACEMENT_3D('',#18460,#15022,#15023);
#13303=AXIS2_PLACEMENT_3D('',#18461,#15024,#15025);
#13304=AXIS2_PLACEMENT_3D('',#18462,#15026,#15027);
#13305=AXIS2_PLACEMENT_3D('',#18465,#15028,#15029);
#13306=AXIS2_PLACEMENT_3D('',#18469,#15031,#15032);
#13307=AXIS2_PLACEMENT_3D('',#18471,#15034,#15035);
#13308=AXIS2_PLACEMENT_3D('',#18480,#15040,#15041);
#13309=AXIS2_PLACEMENT_3D('',#18482,#15042,#15043);
#13310=AXIS2_PLACEMENT_3D('',#18483,#15044,#15045);
#13311=AXIS2_PLACEMENT_3D('',#18496,#15052,#15053);
#13312=AXIS2_PLACEMENT_3D('',#18498,#15054,#15055);
#13313=AXIS2_PLACEMENT_3D('',#18500,#15056,#15057);
#13314=AXIS2_PLACEMENT_3D('',#18502,#15058,#15059);
#13315=AXIS2_PLACEMENT_3D('',#18504,#15060,#15061);
#13316=AXIS2_PLACEMENT_3D('',#18505,#15062,#15063);
#13317=AXIS2_PLACEMENT_3D('',#18508,#15065,#15066);
#13318=AXIS2_PLACEMENT_3D('',#18509,#15067,#15068);
#13319=AXIS2_PLACEMENT_3D('',#18512,#15070,#15071);
#13320=AXIS2_PLACEMENT_3D('',#18513,#15072,#15073);
#13321=AXIS2_PLACEMENT_3D('',#18516,#15075,#15076);
#13322=AXIS2_PLACEMENT_3D('',#18517,#15077,#15078);
#13323=AXIS2_PLACEMENT_3D('',#18520,#15080,#15081);
#13324=AXIS2_PLACEMENT_3D('',#18521,#15082,#15083);
#13325=AXIS2_PLACEMENT_3D('',#18524,#15085,#15086);
#13326=AXIS2_PLACEMENT_3D('',#18525,#15087,#15088);
#13327=AXIS2_PLACEMENT_3D('',#18528,#15090,#15091);
#13328=AXIS2_PLACEMENT_3D('',#18529,#15092,#15093);
#13329=AXIS2_PLACEMENT_3D('',#18532,#15095,#15096);
#13330=AXIS2_PLACEMENT_3D('',#18533,#15097,#15098);
#13331=AXIS2_PLACEMENT_3D('',#18539,#15102,#15103);
#13332=AXIS2_PLACEMENT_3D('',#18545,#15107,#15108);
#13333=AXIS2_PLACEMENT_3D('',#18547,#15110,#15111);
#13334=AXIS2_PLACEMENT_3D('',#18549,#15113,#15114);
#13335=AXIS2_PLACEMENT_3D('',#18553,#15117,#15118);
#13336=AXIS2_PLACEMENT_3D('',#18557,#15121,#15122);
#13337=AXIS2_PLACEMENT_3D('',#18559,#15124,#15125);
#13338=AXIS2_PLACEMENT_3D('',#18560,#15126,#15127);
#13339=AXIS2_PLACEMENT_3D('',#18561,#15128,#15129);
#13340=AXIS2_PLACEMENT_3D('',#18563,#15130,#15131);
#13341=AXIS2_PLACEMENT_3D('',#18566,#15133,#15134);
#13342=AXIS2_PLACEMENT_3D('',#18567,#15135,#15136);
#13343=AXIS2_PLACEMENT_3D('',#18569,#15137,#15138);
#13344=AXIS2_PLACEMENT_3D('',#18572,#15140,#15141);
#13345=AXIS2_PLACEMENT_3D('',#18573,#15142,#15143);
#13346=AXIS2_PLACEMENT_3D('',#18575,#15144,#15145);
#13347=AXIS2_PLACEMENT_3D('',#18578,#15147,#15148);
#13348=AXIS2_PLACEMENT_3D('',#18579,#15149,#15150);
#13349=AXIS2_PLACEMENT_3D('',#18581,#15151,#15152);
#13350=AXIS2_PLACEMENT_3D('',#18584,#15154,#15155);
#13351=AXIS2_PLACEMENT_3D('',#18585,#15156,#15157);
#13352=AXIS2_PLACEMENT_3D('',#18587,#15158,#15159);
#13353=AXIS2_PLACEMENT_3D('',#18590,#15161,#15162);
#13354=AXIS2_PLACEMENT_3D('',#18591,#15163,#15164);
#13355=AXIS2_PLACEMENT_3D('',#18593,#15165,#15166);
#13356=AXIS2_PLACEMENT_3D('',#18596,#15168,#15169);
#13357=AXIS2_PLACEMENT_3D('',#18597,#15170,#15171);
#13358=AXIS2_PLACEMENT_3D('',#18598,#15172,#15173);
#13359=AXIS2_PLACEMENT_3D('',#18600,#15174,#15175);
#13360=AXIS2_PLACEMENT_3D('',#18603,#15177,#15178);
#13361=AXIS2_PLACEMENT_3D('',#18604,#15179,#15180);
#13362=AXIS2_PLACEMENT_3D('',#18605,#15181,#15182);
#13363=AXIS2_PLACEMENT_3D('',#18606,#15183,#15184);
#13364=AXIS2_PLACEMENT_3D('',#18607,#15185,#15186);
#13365=AXIS2_PLACEMENT_3D('',#18609,#15187,#15188);
#13366=AXIS2_PLACEMENT_3D('',#18612,#15190,#15191);
#13367=AXIS2_PLACEMENT_3D('',#18613,#15192,#15193);
#13368=AXIS2_PLACEMENT_3D('',#18615,#15194,#15195);
#13369=AXIS2_PLACEMENT_3D('',#18618,#15197,#15198);
#13370=AXIS2_PLACEMENT_3D('',#18619,#15199,#15200);
#13371=AXIS2_PLACEMENT_3D('',#18621,#15201,#15202);
#13372=AXIS2_PLACEMENT_3D('',#18624,#15204,#15205);
#13373=AXIS2_PLACEMENT_3D('',#18625,#15206,#15207);
#13374=AXIS2_PLACEMENT_3D('',#18627,#15208,#15209);
#13375=AXIS2_PLACEMENT_3D('',#18630,#15211,#15212);
#13376=AXIS2_PLACEMENT_3D('',#18631,#15213,#15214);
#13377=AXIS2_PLACEMENT_3D('',#18633,#15215,#15216);
#13378=AXIS2_PLACEMENT_3D('',#18636,#15218,#15219);
#13379=AXIS2_PLACEMENT_3D('',#18637,#15220,#15221);
#13380=AXIS2_PLACEMENT_3D('',#18639,#15222,#15223);
#13381=AXIS2_PLACEMENT_3D('',#18642,#15225,#15226);
#13382=AXIS2_PLACEMENT_3D('',#18643,#15227,#15228);
#13383=AXIS2_PLACEMENT_3D('',#18644,#15229,#15230);
#13384=AXIS2_PLACEMENT_3D('',#18646,#15231,#15232);
#13385=AXIS2_PLACEMENT_3D('',#18649,#15234,#15235);
#13386=AXIS2_PLACEMENT_3D('',#18650,#15236,#15237);
#13387=AXIS2_PLACEMENT_3D('',#18651,#15238,#15239);
#13388=AXIS2_PLACEMENT_3D('',#18652,#15240,#15241);
#13389=AXIS2_PLACEMENT_3D('',#18653,#15242,#15243);
#13390=AXIS2_PLACEMENT_3D('',#18655,#15244,#15245);
#13391=AXIS2_PLACEMENT_3D('',#18656,#15246,#15247);
#13392=AXIS2_PLACEMENT_3D('',#18658,#15248,#15249);
#13393=AXIS2_PLACEMENT_3D('',#18660,#15251,#15252);
#13394=AXIS2_PLACEMENT_3D('',#18662,#15253,#15254);
#13395=AXIS2_PLACEMENT_3D('',#18664,#15256,#15257);
#13396=AXIS2_PLACEMENT_3D('',#18666,#15258,#15259);
#13397=AXIS2_PLACEMENT_3D('',#18668,#15261,#15262);
#13398=AXIS2_PLACEMENT_3D('',#18670,#15263,#15264);
#13399=AXIS2_PLACEMENT_3D('',#18671,#15265,#15266);
#13400=AXIS2_PLACEMENT_3D('',#18673,#15267,#15268);
#13401=AXIS2_PLACEMENT_3D('',#18675,#15270,#15271);
#13402=AXIS2_PLACEMENT_3D('',#18677,#15272,#15273);
#13403=AXIS2_PLACEMENT_3D('',#18679,#15275,#15276);
#13404=AXIS2_PLACEMENT_3D('',#18681,#15277,#15278);
#13405=AXIS2_PLACEMENT_3D('',#18683,#15280,#15281);
#13406=AXIS2_PLACEMENT_3D('',#18684,#15282,#15283);
#13407=AXIS2_PLACEMENT_3D('',#18693,#15288,#15289);
#13408=AXIS2_PLACEMENT_3D('',#18699,#15293,#15294);
#13409=AXIS2_PLACEMENT_3D('',#18705,#15298,#15299);
#13410=AXIS2_PLACEMENT_3D('',#18711,#15303,#15304);
#13411=AXIS2_PLACEMENT_3D('',#18717,#15308,#15309);
#13412=AXIS2_PLACEMENT_3D('',#18720,#15312,#15313);
#13413=AXIS2_PLACEMENT_3D('',#18721,#15314,#15315);
#13414=AXIS2_PLACEMENT_3D('',#18722,#15316,#15317);
#13415=AXIS2_PLACEMENT_3D('',#18723,#15318,#15319);
#13416=AXIS2_PLACEMENT_3D('',#18724,#15320,#15321);
#13417=AXIS2_PLACEMENT_3D('',#18727,#15322,#15323);
#13418=AXIS2_PLACEMENT_3D('',#18728,#15324,#15325);
#13419=AXIS2_PLACEMENT_3D('',#18730,#15326,#15327);
#13420=AXIS2_PLACEMENT_3D('',#18732,#15328,#15329);
#13421=AXIS2_PLACEMENT_3D('',#18733,#15330,#15331);
#13422=AXIS2_PLACEMENT_3D('',#18734,#15332,#15333);
#13423=AXIS2_PLACEMENT_3D('',#18737,#15335,#15336);
#13424=AXIS2_PLACEMENT_3D('',#18738,#15337,#15338);
#13425=AXIS2_PLACEMENT_3D('',#18740,#15339,#15340);
#13426=AXIS2_PLACEMENT_3D('',#18743,#15342,#15343);
#13427=AXIS2_PLACEMENT_3D('',#18744,#15344,#15345);
#13428=AXIS2_PLACEMENT_3D('',#18747,#15347,#15348);
#13429=AXIS2_PLACEMENT_3D('',#18748,#15349,#15350);
#13430=AXIS2_PLACEMENT_3D('',#18749,#15351,#15352);
#13431=AXIS2_PLACEMENT_3D('',#18751,#15353,#15354);
#13432=AXIS2_PLACEMENT_3D('',#18753,#15356,#15357);
#13433=AXIS2_PLACEMENT_3D('',#18755,#15358,#15359);
#13434=AXIS2_PLACEMENT_3D('',#18756,#15360,#15361);
#13435=AXIS2_PLACEMENT_3D('',#18758,#15363,#15364);
#13436=AXIS2_PLACEMENT_3D('',#18759,#15365,#15366);
#13437=AXIS2_PLACEMENT_3D('',#18762,#15367,#15368);
#13438=AXIS2_PLACEMENT_3D('',#18763,#15369,#15370);
#13439=AXIS2_PLACEMENT_3D('',#18765,#15371,#15372);
#13440=AXIS2_PLACEMENT_3D('',#18767,#15373,#15374);
#13441=AXIS2_PLACEMENT_3D('',#18768,#15375,#15376);
#13442=AXIS2_PLACEMENT_3D('',#18769,#15377,#15378);
#13443=AXIS2_PLACEMENT_3D('',#18771,#15379,#15380);
#13444=AXIS2_PLACEMENT_3D('',#18773,#15382,#15383);
#13445=AXIS2_PLACEMENT_3D('',#18775,#15384,#15385);
#13446=AXIS2_PLACEMENT_3D('',#18777,#15386,#15387);
#13447=AXIS2_PLACEMENT_3D('',#18778,#15388,#15389);
#13448=AXIS2_PLACEMENT_3D('',#18780,#15390,#15391);
#13449=AXIS2_PLACEMENT_3D('',#18782,#15393,#15394);
#13450=AXIS2_PLACEMENT_3D('',#18784,#15395,#15396);
#13451=AXIS2_PLACEMENT_3D('',#18786,#15398,#15399);
#13452=AXIS2_PLACEMENT_3D('',#18788,#15400,#15401);
#13453=AXIS2_PLACEMENT_3D('',#18790,#15403,#15404);
#13454=AXIS2_PLACEMENT_3D('',#18791,#15405,#15406);
#13455=AXIS2_PLACEMENT_3D('',#18793,#15408,#15409);
#13456=AXIS2_PLACEMENT_3D('',#18794,#15410,#15411);
#13457=AXIS2_PLACEMENT_3D('',#18797,#15412,#15413);
#13458=AXIS2_PLACEMENT_3D('',#18798,#15414,#15415);
#13459=AXIS2_PLACEMENT_3D('',#18801,#15416,#15417);
#13460=AXIS2_PLACEMENT_3D('',#18802,#15418,#15419);
#13461=AXIS2_PLACEMENT_3D('',#18805,#15420,#15421);
#13462=AXIS2_PLACEMENT_3D('',#18806,#15422,#15423);
#13463=AXIS2_PLACEMENT_3D('',#18809,#15424,#15425);
#13464=AXIS2_PLACEMENT_3D('',#18810,#15426,#15427);
#13465=AXIS2_PLACEMENT_3D('',#18813,#15428,#15429);
#13466=AXIS2_PLACEMENT_3D('',#18814,#15430,#15431);
#13467=AXIS2_PLACEMENT_3D('',#18817,#15432,#15433);
#13468=AXIS2_PLACEMENT_3D('',#18818,#15434,#15435);
#13469=AXIS2_PLACEMENT_3D('',#18821,#15436,#15437);
#13470=AXIS2_PLACEMENT_3D('',#18822,#15438,#15439);
#13471=AXIS2_PLACEMENT_3D('',#18823,#15440,#15441);
#13472=AXIS2_PLACEMENT_3D('',#18849,#15442,#15443);
#13473=AXIS2_PLACEMENT_3D('',#18873,#15444,#15445);
#13474=AXIS2_PLACEMENT_3D('',#18874,#15446,#15447);
#13475=AXIS2_PLACEMENT_3D('',#18876,#15448,#15449);
#13476=AXIS2_PLACEMENT_3D('',#18901,#15450,#15451);
#13477=AXIS2_PLACEMENT_3D('',#18926,#15452,#15453);
#13478=AXIS2_PLACEMENT_3D('',#18929,#15455,#15456);
#13479=AXIS2_PLACEMENT_3D('',#18931,#15457,#15458);
#13480=AXIS2_PLACEMENT_3D('',#18956,#15459,#15460);
#13481=AXIS2_PLACEMENT_3D('',#18981,#15461,#15462);
#13482=AXIS2_PLACEMENT_3D('',#19006,#15463,#15464);
#13483=AXIS2_PLACEMENT_3D('',#19030,#15465,#15466);
#13484=AXIS2_PLACEMENT_3D('',#19031,#15467,#15468);
#13485=AXIS2_PLACEMENT_3D('',#19033,#15469,#15470);
#13486=AXIS2_PLACEMENT_3D('',#19034,#15471,#15472);
#13487=AXIS2_PLACEMENT_3D('',#19035,#15473,#15474);
#13488=AXIS2_PLACEMENT_3D('',#19059,#15475,#15476);
#13489=AXIS2_PLACEMENT_3D('',#19060,#15477,#15478);
#13490=AXIS2_PLACEMENT_3D('',#19062,#15479,#15480);
#13491=AXIS2_PLACEMENT_3D('',#19063,#15481,#15482);
#13492=AXIS2_PLACEMENT_3D('',#19064,#15483,#15484);
#13493=AXIS2_PLACEMENT_3D('',#19088,#15485,#15486);
#13494=AXIS2_PLACEMENT_3D('',#19089,#15487,#15488);
#13495=AXIS2_PLACEMENT_3D('',#19091,#15489,#15490);
#13496=AXIS2_PLACEMENT_3D('',#19093,#15491,#15492);
#13497=AXIS2_PLACEMENT_3D('',#19094,#15493,#15494);
#13498=AXIS2_PLACEMENT_3D('',#19095,#15495,#15496);
#13499=AXIS2_PLACEMENT_3D('',#19119,#15497,#15498);
#13500=AXIS2_PLACEMENT_3D('',#19120,#15499,#15500);
#13501=AXIS2_PLACEMENT_3D('',#19122,#15501,#15502);
#13502=AXIS2_PLACEMENT_3D('',#19123,#15503,#15504);
#13503=AXIS2_PLACEMENT_3D('',#19124,#15505,#15506);
#13504=AXIS2_PLACEMENT_3D('',#19148,#15507,#15508);
#13505=AXIS2_PLACEMENT_3D('',#19149,#15509,#15510);
#13506=AXIS2_PLACEMENT_3D('',#19151,#15511,#15512);
#13507=AXIS2_PLACEMENT_3D('',#19152,#15513,#15514);
#13508=AXIS2_PLACEMENT_3D('',#19153,#15515,#15516);
#13509=AXIS2_PLACEMENT_3D('',#19177,#15517,#15518);
#13510=AXIS2_PLACEMENT_3D('',#19178,#15519,#15520);
#13511=AXIS2_PLACEMENT_3D('',#19180,#15521,#15522);
#13512=AXIS2_PLACEMENT_3D('',#19183,#15524,#15525);
#13513=AXIS2_PLACEMENT_3D('',#19207,#15526,#15527);
#13514=AXIS2_PLACEMENT_3D('',#19208,#15528,#15529);
#13515=AXIS2_PLACEMENT_3D('',#19209,#15530,#15531);
#13516=AXIS2_PLACEMENT_3D('',#19210,#15532,#15533);
#13517=AXIS2_PLACEMENT_3D('',#19211,#15534,#15535);
#13518=AXIS2_PLACEMENT_3D('',#19212,#15536,#15537);
#13519=AXIS2_PLACEMENT_3D('',#19213,#15538,#15539);
#13520=AXIS2_PLACEMENT_3D('',#19214,#15540,#15541);
#13521=AXIS2_PLACEMENT_3D('',#19215,#15542,#15543);
#13522=AXIS2_PLACEMENT_3D('',#19217,#15544,#15545);
#13523=AXIS2_PLACEMENT_3D('',#19219,#15546,#15547);
#13524=AXIS2_PLACEMENT_3D('',#19220,#15548,#15549);
#13525=AXIS2_PLACEMENT_3D('',#19222,#15550,#15551);
#13526=AXIS2_PLACEMENT_3D('',#19224,#15553,#15554);
#13527=AXIS2_PLACEMENT_3D('',#19226,#15555,#15556);
#13528=AXIS2_PLACEMENT_3D('',#19227,#15557,#15558);
#13529=AXIS2_PLACEMENT_3D('',#19229,#15560,#15561);
#13530=AXIS2_PLACEMENT_3D('',#19231,#15562,#15563);
#13531=AXIS2_PLACEMENT_3D('',#19233,#15564,#15565);
#13532=AXIS2_PLACEMENT_3D('',#19234,#15566,#15567);
#13533=AXIS2_PLACEMENT_3D('',#19236,#15568,#15569);
#13534=AXIS2_PLACEMENT_3D('',#19238,#15571,#15572);
#13535=AXIS2_PLACEMENT_3D('',#19240,#15573,#15574);
#13536=AXIS2_PLACEMENT_3D('',#19241,#15575,#15576);
#13537=AXIS2_PLACEMENT_3D('',#19243,#15578,#15579);
#13538=AXIS2_PLACEMENT_3D('',#19244,#15580,#15581);
#13539=AXIS2_PLACEMENT_3D('',#19245,#15582,#15583);
#13540=AXIS2_PLACEMENT_3D('',#19246,#15584,#15585);
#13541=AXIS2_PLACEMENT_3D('',#19247,#15586,#15587);
#13542=AXIS2_PLACEMENT_3D('',#19248,#15588,#15589);
#13543=AXIS2_PLACEMENT_3D('',#19249,#15590,#15591);
#13544=AXIS2_PLACEMENT_3D('',#19258,#15596,#15597);
#13545=AXIS2_PLACEMENT_3D('',#19264,#15601,#15602);
#13546=AXIS2_PLACEMENT_3D('',#19270,#15606,#15607);
#13547=AXIS2_PLACEMENT_3D('',#19276,#15611,#15612);
#13548=AXIS2_PLACEMENT_3D('',#19282,#15616,#15617);
#13549=AXIS2_PLACEMENT_3D('',#19285,#15620,#15621);
#13550=AXIS2_PLACEMENT_3D('',#19286,#15622,#15623);
#13551=AXIS2_PLACEMENT_3D('',#19287,#15624,#15625);
#13552=AXIS2_PLACEMENT_3D('',#19289,#15626,#15627);
#13553=AXIS2_PLACEMENT_3D('',#19290,#15628,#15629);
#13554=AXIS2_PLACEMENT_3D('',#19292,#15630,#15631);
#13555=AXIS2_PLACEMENT_3D('',#19293,#15632,#15633);
#13556=AXIS2_PLACEMENT_3D('',#19295,#15634,#15635);
#13557=AXIS2_PLACEMENT_3D('',#19297,#15637,#15638);
#13558=AXIS2_PLACEMENT_3D('',#19299,#15639,#15640);
#13559=AXIS2_PLACEMENT_3D('',#19301,#15642,#15643);
#13560=AXIS2_PLACEMENT_3D('',#19303,#15644,#15645);
#13561=AXIS2_PLACEMENT_3D('',#19305,#15647,#15648);
#13562=AXIS2_PLACEMENT_3D('',#19307,#15649,#15650);
#13563=AXIS2_PLACEMENT_3D('',#19308,#15651,#15652);
#13564=AXIS2_PLACEMENT_3D('',#19310,#15653,#15654);
#13565=AXIS2_PLACEMENT_3D('',#19312,#15656,#15657);
#13566=AXIS2_PLACEMENT_3D('',#19314,#15659,#15660);
#13567=AXIS2_PLACEMENT_3D('',#19315,#15661,#15662);
#13568=AXIS2_PLACEMENT_3D('',#19316,#15663,#15664);
#13569=AXIS2_PLACEMENT_3D('',#19318,#15665,#15666);
#13570=AXIS2_PLACEMENT_3D('',#19321,#15668,#15669);
#13571=AXIS2_PLACEMENT_3D('',#19322,#15670,#15671);
#13572=AXIS2_PLACEMENT_3D('',#19323,#15672,#15673);
#13573=AXIS2_PLACEMENT_3D('',#19332,#15678,#15679);
#13574=AXIS2_PLACEMENT_3D('',#19341,#15684,#15685);
#13575=AXIS2_PLACEMENT_3D('',#19343,#15686,#15687);
#13576=AXIS2_PLACEMENT_3D('',#19349,#15691,#15692);
#13577=AXIS2_PLACEMENT_3D('',#19350,#15693,#15694);
#13578=AXIS2_PLACEMENT_3D('',#19352,#15695,#15696);
#13579=AXIS2_PLACEMENT_3D('',#19358,#15700,#15701);
#13580=AXIS2_PLACEMENT_3D('',#19359,#15702,#15703);
#13581=AXIS2_PLACEMENT_3D('',#19365,#15707,#15708);
#13582=AXIS2_PLACEMENT_3D('',#19371,#15712,#15713);
#13583=AXIS2_PLACEMENT_3D('',#19377,#15717,#15718);
#13584=AXIS2_PLACEMENT_3D('',#19383,#15722,#15723);
#13585=AXIS2_PLACEMENT_3D('',#19389,#15727,#15728);
#13586=AXIS2_PLACEMENT_3D('',#19395,#15732,#15733);
#13587=AXIS2_PLACEMENT_3D('',#19401,#15737,#15738);
#13588=AXIS2_PLACEMENT_3D('',#19407,#15742,#15743);
#13589=AXIS2_PLACEMENT_3D('',#19413,#15747,#15748);
#13590=AXIS2_PLACEMENT_3D('',#19419,#15752,#15753);
#13591=AXIS2_PLACEMENT_3D('',#19425,#15757,#15758);
#13592=AXIS2_PLACEMENT_3D('',#19431,#15762,#15763);
#13593=AXIS2_PLACEMENT_3D('',#19437,#15767,#15768);
#13594=AXIS2_PLACEMENT_3D('',#19443,#15772,#15773);
#13595=AXIS2_PLACEMENT_3D('',#19449,#15777,#15778);
#13596=AXIS2_PLACEMENT_3D('',#19455,#15782,#15783);
#13597=AXIS2_PLACEMENT_3D('',#19461,#15787,#15788);
#13598=AXIS2_PLACEMENT_3D('',#19467,#15792,#15793);
#13599=AXIS2_PLACEMENT_3D('',#19473,#15797,#15798);
#13600=AXIS2_PLACEMENT_3D('',#19479,#15802,#15803);
#13601=AXIS2_PLACEMENT_3D('',#19485,#15807,#15808);
#13602=AXIS2_PLACEMENT_3D('',#19491,#15812,#15813);
#13603=AXIS2_PLACEMENT_3D('',#19497,#15817,#15818);
#13604=AXIS2_PLACEMENT_3D('',#19503,#15822,#15823);
#13605=AXIS2_PLACEMENT_3D('',#19509,#15827,#15828);
#13606=AXIS2_PLACEMENT_3D('',#19515,#15832,#15833);
#13607=AXIS2_PLACEMENT_3D('',#19521,#15837,#15838);
#13608=AXIS2_PLACEMENT_3D('',#19527,#15842,#15843);
#13609=AXIS2_PLACEMENT_3D('',#19533,#15847,#15848);
#13610=AXIS2_PLACEMENT_3D('',#19539,#15852,#15853);
#13611=AXIS2_PLACEMENT_3D('',#19545,#15857,#15858);
#13612=AXIS2_PLACEMENT_3D('',#19551,#15862,#15863);
#13613=AXIS2_PLACEMENT_3D('',#19557,#15867,#15868);
#13614=AXIS2_PLACEMENT_3D('',#19563,#15872,#15873);
#13615=AXIS2_PLACEMENT_3D('',#19569,#15877,#15878);
#13616=AXIS2_PLACEMENT_3D('',#19575,#15882,#15883);
#13617=AXIS2_PLACEMENT_3D('',#19581,#15887,#15888);
#13618=AXIS2_PLACEMENT_3D('',#19587,#15892,#15893);
#13619=AXIS2_PLACEMENT_3D('',#19593,#15897,#15898);
#13620=AXIS2_PLACEMENT_3D('',#19599,#15902,#15903);
#13621=AXIS2_PLACEMENT_3D('',#19605,#15907,#15908);
#13622=AXIS2_PLACEMENT_3D('',#19611,#15912,#15913);
#13623=AXIS2_PLACEMENT_3D('',#19617,#15917,#15918);
#13624=AXIS2_PLACEMENT_3D('',#19623,#15922,#15923);
#13625=AXIS2_PLACEMENT_3D('',#19629,#15927,#15928);
#13626=AXIS2_PLACEMENT_3D('',#19635,#15932,#15933);
#13627=AXIS2_PLACEMENT_3D('',#19641,#15937,#15938);
#13628=AXIS2_PLACEMENT_3D('',#19647,#15942,#15943);
#13629=AXIS2_PLACEMENT_3D('',#19653,#15947,#15948);
#13630=AXIS2_PLACEMENT_3D('',#19659,#15952,#15953);
#13631=AXIS2_PLACEMENT_3D('',#19665,#15957,#15958);
#13632=AXIS2_PLACEMENT_3D('',#19671,#15962,#15963);
#13633=AXIS2_PLACEMENT_3D('',#19677,#15967,#15968);
#13634=AXIS2_PLACEMENT_3D('',#19683,#15972,#15973);
#13635=AXIS2_PLACEMENT_3D('',#19689,#15977,#15978);
#13636=AXIS2_PLACEMENT_3D('',#19695,#15982,#15983);
#13637=AXIS2_PLACEMENT_3D('',#19701,#15987,#15988);
#13638=AXIS2_PLACEMENT_3D('',#19707,#15992,#15993);
#13639=AXIS2_PLACEMENT_3D('',#19713,#15997,#15998);
#13640=AXIS2_PLACEMENT_3D('',#19719,#16002,#16003);
#13641=AXIS2_PLACEMENT_3D('',#19725,#16007,#16008);
#13642=AXIS2_PLACEMENT_3D('',#19731,#16012,#16013);
#13643=AXIS2_PLACEMENT_3D('',#19737,#16017,#16018);
#13644=AXIS2_PLACEMENT_3D('',#19743,#16022,#16023);
#13645=AXIS2_PLACEMENT_3D('',#19749,#16027,#16028);
#13646=AXIS2_PLACEMENT_3D('',#19755,#16032,#16033);
#13647=AXIS2_PLACEMENT_3D('',#19761,#16037,#16038);
#13648=AXIS2_PLACEMENT_3D('',#19767,#16042,#16043);
#13649=AXIS2_PLACEMENT_3D('',#19773,#16047,#16048);
#13650=AXIS2_PLACEMENT_3D('',#19779,#16052,#16053);
#13651=AXIS2_PLACEMENT_3D('',#19785,#16057,#16058);
#13652=AXIS2_PLACEMENT_3D('',#19791,#16062,#16063);
#13653=AXIS2_PLACEMENT_3D('',#19797,#16067,#16068);
#13654=AXIS2_PLACEMENT_3D('',#19803,#16072,#16073);
#13655=AXIS2_PLACEMENT_3D('',#19809,#16077,#16078);
#13656=AXIS2_PLACEMENT_3D('',#19815,#16082,#16083);
#13657=AXIS2_PLACEMENT_3D('',#19821,#16087,#16088);
#13658=AXIS2_PLACEMENT_3D('',#19827,#16092,#16093);
#13659=AXIS2_PLACEMENT_3D('',#19833,#16097,#16098);
#13660=AXIS2_PLACEMENT_3D('',#19839,#16102,#16103);
#13661=AXIS2_PLACEMENT_3D('',#19845,#16107,#16108);
#13662=AXIS2_PLACEMENT_3D('',#19851,#16112,#16113);
#13663=AXIS2_PLACEMENT_3D('',#19857,#16117,#16118);
#13664=AXIS2_PLACEMENT_3D('',#19863,#16122,#16123);
#13665=AXIS2_PLACEMENT_3D('',#19869,#16127,#16128);
#13666=AXIS2_PLACEMENT_3D('',#19875,#16132,#16133);
#13667=AXIS2_PLACEMENT_3D('',#19881,#16137,#16138);
#13668=AXIS2_PLACEMENT_3D('',#19887,#16142,#16143);
#13669=AXIS2_PLACEMENT_3D('',#19893,#16147,#16148);
#13670=AXIS2_PLACEMENT_3D('',#19899,#16152,#16153);
#13671=AXIS2_PLACEMENT_3D('',#19905,#16157,#16158);
#13672=AXIS2_PLACEMENT_3D('',#19911,#16162,#16163);
#13673=AXIS2_PLACEMENT_3D('',#19917,#16167,#16168);
#13674=AXIS2_PLACEMENT_3D('',#19923,#16172,#16173);
#13675=AXIS2_PLACEMENT_3D('',#19929,#16177,#16178);
#13676=AXIS2_PLACEMENT_3D('',#19935,#16182,#16183);
#13677=AXIS2_PLACEMENT_3D('',#19941,#16187,#16188);
#13678=AXIS2_PLACEMENT_3D('',#19947,#16192,#16193);
#13679=AXIS2_PLACEMENT_3D('',#19953,#16197,#16198);
#13680=AXIS2_PLACEMENT_3D('',#19959,#16202,#16203);
#13681=AXIS2_PLACEMENT_3D('',#19965,#16207,#16208);
#13682=AXIS2_PLACEMENT_3D('',#19971,#16212,#16213);
#13683=AXIS2_PLACEMENT_3D('',#19977,#16217,#16218);
#13684=AXIS2_PLACEMENT_3D('',#19983,#16222,#16223);
#13685=AXIS2_PLACEMENT_3D('',#19989,#16227,#16228);
#13686=AXIS2_PLACEMENT_3D('',#19995,#16232,#16233);
#13687=AXIS2_PLACEMENT_3D('',#20001,#16237,#16238);
#13688=AXIS2_PLACEMENT_3D('',#20007,#16242,#16243);
#13689=AXIS2_PLACEMENT_3D('',#20013,#16247,#16248);
#13690=AXIS2_PLACEMENT_3D('',#20019,#16252,#16253);
#13691=AXIS2_PLACEMENT_3D('',#20025,#16257,#16258);
#13692=AXIS2_PLACEMENT_3D('',#20031,#16262,#16263);
#13693=AXIS2_PLACEMENT_3D('',#20037,#16267,#16268);
#13694=AXIS2_PLACEMENT_3D('',#20043,#16272,#16273);
#13695=AXIS2_PLACEMENT_3D('',#20049,#16277,#16278);
#13696=AXIS2_PLACEMENT_3D('',#20055,#16282,#16283);
#13697=AXIS2_PLACEMENT_3D('',#20061,#16287,#16288);
#13698=AXIS2_PLACEMENT_3D('',#20067,#16292,#16293);
#13699=AXIS2_PLACEMENT_3D('',#20073,#16297,#16298);
#13700=AXIS2_PLACEMENT_3D('',#20079,#16302,#16303);
#13701=AXIS2_PLACEMENT_3D('',#20085,#16307,#16308);
#13702=AXIS2_PLACEMENT_3D('',#20091,#16312,#16313);
#13703=AXIS2_PLACEMENT_3D('',#20097,#16317,#16318);
#13704=AXIS2_PLACEMENT_3D('',#20103,#16322,#16323);
#13705=AXIS2_PLACEMENT_3D('',#20109,#16327,#16328);
#13706=AXIS2_PLACEMENT_3D('',#20115,#16332,#16333);
#13707=AXIS2_PLACEMENT_3D('',#20121,#16337,#16338);
#13708=AXIS2_PLACEMENT_3D('',#20127,#16342,#16343);
#13709=AXIS2_PLACEMENT_3D('',#20133,#16347,#16348);
#13710=AXIS2_PLACEMENT_3D('',#20139,#16352,#16353);
#13711=AXIS2_PLACEMENT_3D('',#20145,#16357,#16358);
#13712=AXIS2_PLACEMENT_3D('',#20151,#16362,#16363);
#13713=AXIS2_PLACEMENT_3D('',#20157,#16367,#16368);
#13714=AXIS2_PLACEMENT_3D('',#20163,#16372,#16373);
#13715=AXIS2_PLACEMENT_3D('',#20169,#16377,#16378);
#13716=AXIS2_PLACEMENT_3D('',#20175,#16382,#16383);
#13717=AXIS2_PLACEMENT_3D('',#20181,#16387,#16388);
#13718=AXIS2_PLACEMENT_3D('',#20187,#16392,#16393);
#13719=AXIS2_PLACEMENT_3D('',#20193,#16397,#16398);
#13720=AXIS2_PLACEMENT_3D('',#20199,#16402,#16403);
#13721=AXIS2_PLACEMENT_3D('',#20205,#16407,#16408);
#13722=AXIS2_PLACEMENT_3D('',#20211,#16412,#16413);
#13723=AXIS2_PLACEMENT_3D('',#20217,#16417,#16418);
#13724=AXIS2_PLACEMENT_3D('',#20223,#16422,#16423);
#13725=AXIS2_PLACEMENT_3D('',#20229,#16427,#16428);
#13726=AXIS2_PLACEMENT_3D('',#20235,#16432,#16433);
#13727=AXIS2_PLACEMENT_3D('',#20241,#16437,#16438);
#13728=AXIS2_PLACEMENT_3D('',#20247,#16442,#16443);
#13729=AXIS2_PLACEMENT_3D('',#20253,#16447,#16448);
#13730=AXIS2_PLACEMENT_3D('',#20259,#16452,#16453);
#13731=AXIS2_PLACEMENT_3D('',#20265,#16457,#16458);
#13732=AXIS2_PLACEMENT_3D('',#20271,#16462,#16463);
#13733=AXIS2_PLACEMENT_3D('',#20277,#16467,#16468);
#13734=AXIS2_PLACEMENT_3D('',#20283,#16472,#16473);
#13735=AXIS2_PLACEMENT_3D('',#20289,#16477,#16478);
#13736=AXIS2_PLACEMENT_3D('',#20295,#16482,#16483);
#13737=AXIS2_PLACEMENT_3D('',#20301,#16487,#16488);
#13738=AXIS2_PLACEMENT_3D('',#20307,#16492,#16493);
#13739=AXIS2_PLACEMENT_3D('',#20313,#16497,#16498);
#13740=AXIS2_PLACEMENT_3D('',#20319,#16502,#16503);
#13741=AXIS2_PLACEMENT_3D('',#20322,#16506,#16507);
#13742=AXIS2_PLACEMENT_3D('',#20323,#16508,#16509);
#13743=AXIS2_PLACEMENT_3D('',#20324,#16510,#16511);
#13744=AXIS2_PLACEMENT_3D('',#20326,#16512,#16513);
#13745=AXIS2_PLACEMENT_3D('',#20330,#16516,#16517);
#13746=AXIS2_PLACEMENT_3D('',#20331,#16518,#16519);
#13747=AXIS2_PLACEMENT_3D('',#20332,#16520,#16521);
#13748=AXIS2_PLACEMENT_3D('',#20333,#16522,#16523);
#13749=AXIS2_PLACEMENT_3D('',#20334,#16524,#16525);
#13750=AXIS2_PLACEMENT_3D('',#20336,#16526,#16527);
#13751=AXIS2_PLACEMENT_3D('',#20339,#16529,#16530);
#13752=AXIS2_PLACEMENT_3D('',#20340,#16531,#16532);
#13753=AXIS2_PLACEMENT_3D('',#20341,#16533,#16534);
#13754=AXIS2_PLACEMENT_3D('',#20343,#16535,#16536);
#13755=AXIS2_PLACEMENT_3D('',#20346,#16538,#16539);
#13756=AXIS2_PLACEMENT_3D('',#20347,#16540,#16541);
#13757=AXIS2_PLACEMENT_3D('',#20348,#16542,#16543);
#13758=AXIS2_PLACEMENT_3D('',#20349,#16544,#16545);
#13759=AXIS2_PLACEMENT_3D('',#20350,#16546,#16547);
#13760=AXIS2_PLACEMENT_3D('',#20428,#16549,#16550);
#13761=AXIS2_PLACEMENT_3D('',#20437,#16555,#16556);
#13762=AXIS2_PLACEMENT_3D('',#20446,#16561,#16562);
#13763=AXIS2_PLACEMENT_3D('',#20452,#16566,#16567);
#13764=AXIS2_PLACEMENT_3D('',#20458,#16571,#16572);
#13765=AXIS2_PLACEMENT_3D('',#20459,#16573,#16574);
#13766=AXIS2_PLACEMENT_3D('',#20460,#16575,#16576);
#13767=AXIS2_PLACEMENT_3D('',#20461,#16577,#16578);
#13768=AXIS2_PLACEMENT_3D('',#20462,#16579,#16580);
#13769=AXIS2_PLACEMENT_3D('',#20463,#16581,#16582);
#13770=AXIS2_PLACEMENT_3D('',#20464,#16583,#16584);
#13771=AXIS2_PLACEMENT_3D('',#20465,#16585,#16586);
#13772=AXIS2_PLACEMENT_3D('',#20466,#16587,#16588);
#13773=AXIS2_PLACEMENT_3D('',#20467,#16589,#16590);
#13774=AXIS2_PLACEMENT_3D('',#20476,#16595,#16596);
#13775=AXIS2_PLACEMENT_3D('',#20482,#16600,#16601);
#13776=AXIS2_PLACEMENT_3D('',#20488,#16605,#16606);
#13777=AXIS2_PLACEMENT_3D('',#20494,#16610,#16611);
#13778=AXIS2_PLACEMENT_3D('',#20500,#16615,#16616);
#13779=AXIS2_PLACEMENT_3D('',#20503,#16619,#16620);
#13780=AXIS2_PLACEMENT_3D('',#20504,#16621,#16622);
#13781=AXIS2_PLACEMENT_3D('',#20506,#16623,#16624);
#13782=AXIS2_PLACEMENT_3D('',#20507,#16625,#16626);
#13783=AXIS2_PLACEMENT_3D('',#20509,#16627,#16628);
#13784=AXIS2_PLACEMENT_3D('',#20511,#16630,#16631);
#13785=AXIS2_PLACEMENT_3D('',#20513,#16632,#16633);
#13786=AXIS2_PLACEMENT_3D('',#20515,#16635,#16636);
#13787=AXIS2_PLACEMENT_3D('',#20517,#16637,#16638);
#13788=AXIS2_PLACEMENT_3D('',#20519,#16640,#16641);
#13789=AXIS2_PLACEMENT_3D('',#20520,#16642,#16643);
#13790=AXIS2_PLACEMENT_3D('',#20521,#16644,#16645);
#13791=AXIS2_PLACEMENT_3D('',#20522,#16646,#16647);
#13792=AXIS2_PLACEMENT_3D('',#20523,#16648,#16649);
#13793=AXIS2_PLACEMENT_3D('',#20524,#16650,#16651);
#13794=AXIS2_PLACEMENT_3D('',#20525,#16652,#16653);
#13795=AXIS2_PLACEMENT_3D('',#20526,#16654,#16655);
#13796=AXIS2_PLACEMENT_3D('',#20528,#16656,#16657);
#13797=AXIS2_PLACEMENT_3D('',#20531,#16659,#16660);
#13798=AXIS2_PLACEMENT_3D('',#20532,#16661,#16662);
#13799=AXIS2_PLACEMENT_3D('',#20533,#16663,#16664);
#13800=AXIS2_PLACEMENT_3D('',#20535,#16665,#16666);
#13801=AXIS2_PLACEMENT_3D('',#20538,#16668,#16669);
#13802=AXIS2_PLACEMENT_3D('',#20539,#16670,#16671);
#13803=AXIS2_PLACEMENT_3D('',#20540,#16672,#16673);
#13804=AXIS2_PLACEMENT_3D('',#20549,#16678,#16679);
#13805=AXIS2_PLACEMENT_3D('',#20551,#16680,#16681);
#13806=AXIS2_PLACEMENT_3D('',#20555,#16684,#16685);
#13807=AXIS2_PLACEMENT_3D('',#20559,#16688,#16689);
#13808=AXIS2_PLACEMENT_3D('',#20563,#16692,#16693);
#13809=AXIS2_PLACEMENT_3D('',#20564,#16694,#16695);
#13810=AXIS2_PLACEMENT_3D('',#20565,#16696,#16697);
#13811=AXIS2_PLACEMENT_3D('',#20574,#16702,#16703);
#13812=AXIS2_PLACEMENT_3D('',#20576,#16704,#16705);
#13813=AXIS2_PLACEMENT_3D('',#20580,#16708,#16709);
#13814=AXIS2_PLACEMENT_3D('',#20584,#16712,#16713);
#13815=AXIS2_PLACEMENT_3D('',#20588,#16716,#16717);
#13816=AXIS2_PLACEMENT_3D('',#20589,#16718,#16719);
#13817=AXIS2_PLACEMENT_3D('',#20590,#16720,#16721);
#13818=AXIS2_PLACEMENT_3D('',#20592,#16722,#16723);
#13819=AXIS2_PLACEMENT_3D('',#20595,#16725,#16726);
#13820=AXIS2_PLACEMENT_3D('',#20596,#16727,#16728);
#13821=AXIS2_PLACEMENT_3D('',#20597,#16729,#16730);
#13822=AXIS2_PLACEMENT_3D('',#20598,#16731,#16732);
#13823=AXIS2_PLACEMENT_3D('',#20599,#16733,#16734);
#13824=AXIS2_PLACEMENT_3D('',#20601,#16735,#16736);
#13825=AXIS2_PLACEMENT_3D('',#20604,#16738,#16739);
#13826=AXIS2_PLACEMENT_3D('',#20605,#16740,#16741);
#13827=AXIS2_PLACEMENT_3D('',#20607,#16742,#16743);
#13828=AXIS2_PLACEMENT_3D('',#20610,#16745,#16746);
#13829=AXIS2_PLACEMENT_3D('',#20611,#16747,#16748);
#13830=AXIS2_PLACEMENT_3D('',#20612,#16749,#16750);
#13831=AXIS2_PLACEMENT_3D('',#20613,#16751,#16752);
#13832=AXIS2_PLACEMENT_3D('',#20614,#16753,#16754);
#13833=AXIS2_PLACEMENT_3D('',#20616,#16755,#16756);
#13834=AXIS2_PLACEMENT_3D('',#20619,#16758,#16759);
#13835=AXIS2_PLACEMENT_3D('',#20620,#16760,#16761);
#13836=AXIS2_PLACEMENT_3D('',#20622,#16762,#16763);
#13837=AXIS2_PLACEMENT_3D('',#20625,#16765,#16766);
#13838=AXIS2_PLACEMENT_3D('',#20626,#16767,#16768);
#13839=AXIS2_PLACEMENT_3D('',#20627,#16769,#16770);
#13840=AXIS2_PLACEMENT_3D('',#20628,#16771,#16772);
#13841=AXIS2_PLACEMENT_3D('',#20629,#16773,#16774);
#13842=AXIS2_PLACEMENT_3D('',#20631,#16775,#16776);
#13843=AXIS2_PLACEMENT_3D('',#20634,#16778,#16779);
#13844=AXIS2_PLACEMENT_3D('',#20635,#16780,#16781);
#13845=AXIS2_PLACEMENT_3D('',#20637,#16782,#16783);
#13846=AXIS2_PLACEMENT_3D('',#20640,#16785,#16786);
#13847=AXIS2_PLACEMENT_3D('',#20641,#16787,#16788);
#13848=AXIS2_PLACEMENT_3D('',#20642,#16789,#16790);
#13849=AXIS2_PLACEMENT_3D('',#20643,#16791,#16792);
#13850=AXIS2_PLACEMENT_3D('',#20644,#16793,#16794);
#13851=AXIS2_PLACEMENT_3D('',#20646,#16795,#16796);
#13852=AXIS2_PLACEMENT_3D('',#20649,#16798,#16799);
#13853=AXIS2_PLACEMENT_3D('',#20650,#16800,#16801);
#13854=AXIS2_PLACEMENT_3D('',#20652,#16802,#16803);
#13855=AXIS2_PLACEMENT_3D('',#20655,#16805,#16806);
#13856=AXIS2_PLACEMENT_3D('',#20656,#16807,#16808);
#13857=AXIS2_PLACEMENT_3D('',#20657,#16809,#16810);
#13858=AXIS2_PLACEMENT_3D('',#20658,#16811,#16812);
#13859=AXIS2_PLACEMENT_3D('',#20659,#16813,#16814);
#13860=AXIS2_PLACEMENT_3D('',#20668,#16819,#16820);
#13861=AXIS2_PLACEMENT_3D('',#20674,#16824,#16825);
#13862=AXIS2_PLACEMENT_3D('',#20680,#16829,#16830);
#13863=AXIS2_PLACEMENT_3D('',#20683,#16833,#16834);
#13864=AXIS2_PLACEMENT_3D('',#20684,#16835,#16836);
#13865=AXIS2_PLACEMENT_3D('',#20685,#16837,#16838);
#13866=AXIS2_PLACEMENT_3D('',#20686,#16839,#16840);
#13867=AXIS2_PLACEMENT_3D('',#20695,#16845,#16846);
#13868=AXIS2_PLACEMENT_3D('',#20701,#16850,#16851);
#13869=AXIS2_PLACEMENT_3D('',#20707,#16855,#16856);
#13870=AXIS2_PLACEMENT_3D('',#20710,#16859,#16860);
#13871=AXIS2_PLACEMENT_3D('',#20711,#16861,#16862);
#13872=AXIS2_PLACEMENT_3D('',#20712,#16863,#16864);
#13873=AXIS2_PLACEMENT_3D('',#20713,#16865,#16866);
#13874=AXIS2_PLACEMENT_3D('',#20715,#16867,#16868);
#13875=AXIS2_PLACEMENT_3D('',#20718,#16870,#16871);
#13876=AXIS2_PLACEMENT_3D('',#20719,#16872,#16873);
#13877=AXIS2_PLACEMENT_3D('',#20728,#16878,#16879);
#13878=AXIS2_PLACEMENT_3D('',#20734,#16883,#16884);
#13879=AXIS2_PLACEMENT_3D('',#20740,#16888,#16889);
#13880=AXIS2_PLACEMENT_3D('',#20742,#16890,#16891);
#13881=AXIS2_PLACEMENT_3D('',#20743,#16892,#16893);
#13882=AXIS2_PLACEMENT_3D('',#20744,#16894,#16895);
#13883=AXIS2_PLACEMENT_3D('',#20745,#16896,#16897);
#13884=AXIS2_PLACEMENT_3D('',#20746,#16898,#16899);
#13885=AXIS2_PLACEMENT_3D('',#20751,#16901,#16902);
#13886=AXIS2_PLACEMENT_3D('',#20754,#16904,#16905);
#13887=AXIS2_PLACEMENT_3D('',#20755,#16906,#16907);
#13888=AXIS2_PLACEMENT_3D('',#20761,#16911,#16912);
#13889=AXIS2_PLACEMENT_3D('',#20764,#16914,#16915);
#13890=AXIS2_PLACEMENT_3D('',#20765,#16916,#16917);
#13891=AXIS2_PLACEMENT_3D('',#20769,#16920,#16921);
#13892=AXIS2_PLACEMENT_3D('',#20770,#16922,#16923);
#13893=AXIS2_PLACEMENT_3D('',#20771,#16924,#16925);
#13894=AXIS2_PLACEMENT_3D('',#20774,#16927,#16928);
#13895=AXIS2_PLACEMENT_3D('',#20775,#16929,#16930);
#13896=AXIS2_PLACEMENT_3D('',#20776,#16931,#16932);
#13897=AXIS2_PLACEMENT_3D('',#20777,#16933,#16934);
#13898=AXIS2_PLACEMENT_3D('',#20779,#16935,#16936);
#13899=AXIS2_PLACEMENT_3D('',#20782,#16938,#16939);
#13900=AXIS2_PLACEMENT_3D('',#20783,#16940,#16941);
#13901=AXIS2_PLACEMENT_3D('',#20785,#16942,#16943);
#13902=AXIS2_PLACEMENT_3D('',#20788,#16945,#16946);
#13903=AXIS2_PLACEMENT_3D('',#20789,#16947,#16948);
#13904=AXIS2_PLACEMENT_3D('',#20790,#16949,#16950);
#13905=AXIS2_PLACEMENT_3D('',#20791,#16951,#16952);
#13906=AXIS2_PLACEMENT_3D('',#20792,#16953,#16954);
#13907=AXIS2_PLACEMENT_3D('',#20794,#16955,#16956);
#13908=AXIS2_PLACEMENT_3D('',#20797,#16958,#16959);
#13909=AXIS2_PLACEMENT_3D('',#20798,#16960,#16961);
#13910=AXIS2_PLACEMENT_3D('',#20800,#16962,#16963);
#13911=AXIS2_PLACEMENT_3D('',#20803,#16965,#16966);
#13912=AXIS2_PLACEMENT_3D('',#20804,#16967,#16968);
#13913=AXIS2_PLACEMENT_3D('',#20805,#16969,#16970);
#13914=AXIS2_PLACEMENT_3D('',#20806,#16971,#16972);
#13915=AXIS2_PLACEMENT_3D('',#20807,#16973,#16974);
#13916=AXIS2_PLACEMENT_3D('',#20809,#16975,#16976);
#13917=AXIS2_PLACEMENT_3D('',#20812,#16978,#16979);
#13918=AXIS2_PLACEMENT_3D('',#20813,#16980,#16981);
#13919=AXIS2_PLACEMENT_3D('',#20815,#16982,#16983);
#13920=AXIS2_PLACEMENT_3D('',#20818,#16985,#16986);
#13921=AXIS2_PLACEMENT_3D('',#20819,#16987,#16988);
#13922=AXIS2_PLACEMENT_3D('',#20820,#16989,#16990);
#13923=AXIS2_PLACEMENT_3D('',#20821,#16991,#16992);
#13924=AXIS2_PLACEMENT_3D('',#20822,#16993,#16994);
#13925=AXIS2_PLACEMENT_3D('',#20831,#16999,#17000);
#13926=AXIS2_PLACEMENT_3D('',#20837,#17004,#17005);
#13927=AXIS2_PLACEMENT_3D('',#20843,#17009,#17010);
#13928=AXIS2_PLACEMENT_3D('',#20846,#17011,#17012);
#13929=AXIS2_PLACEMENT_3D('',#20992,#17014,#17015);
#13930=AXIS2_PLACEMENT_3D('',#21138,#17017,#17018);
#13931=AXIS2_PLACEMENT_3D('',#21284,#17020,#17021);
#13932=AXIS2_PLACEMENT_3D('',#21430,#17023,#17024);
#13933=AXIS2_PLACEMENT_3D('',#21576,#17026,#17027);
#13934=AXIS2_PLACEMENT_3D('',#21722,#17029,#17030);
#13935=AXIS2_PLACEMENT_3D('',#21868,#17032,#17033);
#13936=AXIS2_PLACEMENT_3D('',#22014,#17035,#17036);
#13937=AXIS2_PLACEMENT_3D('',#22160,#17038,#17039);
#13938=AXIS2_PLACEMENT_3D('',#22306,#17041,#17042);
#13939=AXIS2_PLACEMENT_3D('',#22452,#17044,#17045);
#13940=AXIS2_PLACEMENT_3D('',#22598,#17047,#17048);
#13941=AXIS2_PLACEMENT_3D('',#22744,#17050,#17051);
#13942=AXIS2_PLACEMENT_3D('',#22890,#17053,#17054);
#13943=AXIS2_PLACEMENT_3D('',#23036,#17056,#17057);
#13944=AXIS2_PLACEMENT_3D('',#23182,#17059,#17060);
#13945=AXIS2_PLACEMENT_3D('',#23328,#17062,#17063);
#13946=AXIS2_PLACEMENT_3D('',#23474,#17065,#17066);
#13947=AXIS2_PLACEMENT_3D('',#23620,#17068,#17069);
#13948=AXIS2_PLACEMENT_3D('',#23764,#17071,#17072);
#13949=AXIS2_PLACEMENT_3D('',#23765,#17073,#17074);
#13950=AXIS2_PLACEMENT_3D('',#23766,#17075,#17076);
#13951=AXIS2_PLACEMENT_3D('',#23767,#17077,#17078);
#13952=AXIS2_PLACEMENT_3D('',#23769,#17079,#17080);
#13953=AXIS2_PLACEMENT_3D('',#23772,#17082,#17083);
#13954=AXIS2_PLACEMENT_3D('',#23773,#17084,#17085);
#13955=AXIS2_PLACEMENT_3D('',#23988,#17088,#17089);
#13956=AXIS2_PLACEMENT_3D('',#24204,#17093,#17094);
#13957=AXIS2_PLACEMENT_3D('',#24206,#17095,#17096);
#13958=AXIS2_PLACEMENT_3D('',#24420,#17099,#17100);
#13959=AXIS2_PLACEMENT_3D('',#24636,#17104,#17105);
#13960=AXIS2_PLACEMENT_3D('',#24638,#17106,#17107);
#13961=AXIS2_PLACEMENT_3D('',#24852,#17110,#17111);
#13962=AXIS2_PLACEMENT_3D('',#25068,#17115,#17116);
#13963=AXIS2_PLACEMENT_3D('',#25070,#17117,#17118);
#13964=AXIS2_PLACEMENT_3D('',#25284,#17121,#17122);
#13965=AXIS2_PLACEMENT_3D('',#25500,#17126,#17127);
#13966=AXIS2_PLACEMENT_3D('',#25502,#17128,#17129);
#13967=AXIS2_PLACEMENT_3D('',#25716,#17132,#17133);
#13968=AXIS2_PLACEMENT_3D('',#25932,#17137,#17138);
#13969=AXIS2_PLACEMENT_3D('',#25934,#17139,#17140);
#13970=AXIS2_PLACEMENT_3D('',#26148,#17143,#17144);
#13971=AXIS2_PLACEMENT_3D('',#26364,#17148,#17149);
#13972=AXIS2_PLACEMENT_3D('',#26366,#17150,#17151);
#13973=AXIS2_PLACEMENT_3D('',#26580,#17154,#17155);
#13974=AXIS2_PLACEMENT_3D('',#26796,#17159,#17160);
#13975=AXIS2_PLACEMENT_3D('',#26798,#17161,#17162);
#13976=AXIS2_PLACEMENT_3D('',#27012,#17165,#17166);
#13977=AXIS2_PLACEMENT_3D('',#27228,#17170,#17171);
#13978=AXIS2_PLACEMENT_3D('',#27230,#17172,#17173);
#13979=AXIS2_PLACEMENT_3D('',#27444,#17176,#17177);
#13980=AXIS2_PLACEMENT_3D('',#27660,#17181,#17182);
#13981=AXIS2_PLACEMENT_3D('',#27662,#17183,#17184);
#13982=AXIS2_PLACEMENT_3D('',#27876,#17187,#17188);
#13983=AXIS2_PLACEMENT_3D('',#28092,#17192,#17193);
#13984=AXIS2_PLACEMENT_3D('',#28094,#17194,#17195);
#13985=AXIS2_PLACEMENT_3D('',#28308,#17198,#17199);
#13986=AXIS2_PLACEMENT_3D('',#28524,#17203,#17204);
#13987=AXIS2_PLACEMENT_3D('',#28526,#17205,#17206);
#13988=AXIS2_PLACEMENT_3D('',#28740,#17209,#17210);
#13989=AXIS2_PLACEMENT_3D('',#28956,#17214,#17215);
#13990=AXIS2_PLACEMENT_3D('',#28958,#17216,#17217);
#13991=AXIS2_PLACEMENT_3D('',#29172,#17220,#17221);
#13992=AXIS2_PLACEMENT_3D('',#29388,#17225,#17226);
#13993=AXIS2_PLACEMENT_3D('',#29390,#17227,#17228);
#13994=AXIS2_PLACEMENT_3D('',#29604,#17231,#17232);
#13995=AXIS2_PLACEMENT_3D('',#29820,#17236,#17237);
#13996=AXIS2_PLACEMENT_3D('',#29822,#17238,#17239);
#13997=AXIS2_PLACEMENT_3D('',#30036,#17242,#17243);
#13998=AXIS2_PLACEMENT_3D('',#30252,#17247,#17248);
#13999=AXIS2_PLACEMENT_3D('',#30254,#17249,#17250);
#14000=AXIS2_PLACEMENT_3D('',#30468,#17253,#17254);
#14001=AXIS2_PLACEMENT_3D('',#30684,#17258,#17259);
#14002=AXIS2_PLACEMENT_3D('',#30686,#17260,#17261);
#14003=AXIS2_PLACEMENT_3D('',#30900,#17264,#17265);
#14004=AXIS2_PLACEMENT_3D('',#31116,#17269,#17270);
#14005=AXIS2_PLACEMENT_3D('',#31118,#17271,#17272);
#14006=AXIS2_PLACEMENT_3D('',#31332,#17275,#17276);
#14007=AXIS2_PLACEMENT_3D('',#31548,#17280,#17281);
#14008=AXIS2_PLACEMENT_3D('',#31550,#17282,#17283);
#14009=AXIS2_PLACEMENT_3D('',#31764,#17286,#17287);
#14010=AXIS2_PLACEMENT_3D('',#31980,#17291,#17292);
#14011=AXIS2_PLACEMENT_3D('',#31982,#17293,#17294);
#14012=AXIS2_PLACEMENT_3D('',#32196,#17297,#17298);
#14013=AXIS2_PLACEMENT_3D('',#32412,#17302,#17303);
#14014=AXIS2_PLACEMENT_3D('',#32413,#17304,#17305);
#14015=AXIS2_PLACEMENT_3D('',#32414,#17306,#17307);
#14016=AXIS2_PLACEMENT_3D('',#32415,#17308,#17309);
#14017=AXIS2_PLACEMENT_3D('',#32416,#17310,#17311);
#14018=AXIS2_PLACEMENT_3D('',#32418,#17312,#17313);
#14019=AXIS2_PLACEMENT_3D('',#32421,#17315,#17316);
#14020=AXIS2_PLACEMENT_3D('',#32422,#17317,#17318);
#14021=AXIS2_PLACEMENT_3D('',#32424,#17319,#17320);
#14022=AXIS2_PLACEMENT_3D('',#32427,#17322,#17323);
#14023=AXIS2_PLACEMENT_3D('',#32428,#17324,#17325);
#14024=AXIS2_PLACEMENT_3D('',#32429,#17326,#17327);
#14025=AXIS2_PLACEMENT_3D('',#32430,#17328,#17329);
#14026=AXIS2_PLACEMENT_3D('',#32431,#17330,#17331);
#14027=AXIS2_PLACEMENT_3D('',#32433,#17332,#17333);
#14028=AXIS2_PLACEMENT_3D('',#32434,#17334,#17335);
#14029=AXIS2_PLACEMENT_3D('',#32436,#17336,#17337);
#14030=AXIS2_PLACEMENT_3D('',#32438,#17339,#17340);
#14031=AXIS2_PLACEMENT_3D('',#32440,#17341,#17342);
#14032=AXIS2_PLACEMENT_3D('',#32442,#17344,#17345);
#14033=AXIS2_PLACEMENT_3D('',#32444,#17346,#17347);
#14034=AXIS2_PLACEMENT_3D('',#32446,#17349,#17350);
#14035=AXIS2_PLACEMENT_3D('',#32448,#17351,#17352);
#14036=AXIS2_PLACEMENT_3D('',#32449,#17353,#17354);
#14037=AXIS2_PLACEMENT_3D('',#32451,#17355,#17356);
#14038=AXIS2_PLACEMENT_3D('',#32453,#17358,#17359);
#14039=AXIS2_PLACEMENT_3D('',#32455,#17360,#17361);
#14040=AXIS2_PLACEMENT_3D('',#32457,#17363,#17364);
#14041=AXIS2_PLACEMENT_3D('',#32459,#17365,#17366);
#14042=AXIS2_PLACEMENT_3D('',#32461,#17368,#17369);
#14043=AXIS2_PLACEMENT_3D('',#32462,#17370,#17371);
#14044=AXIS2_PLACEMENT_3D('',#32471,#17376,#17377);
#14045=AXIS2_PLACEMENT_3D('',#32477,#17381,#17382);
#14046=AXIS2_PLACEMENT_3D('',#32483,#17386,#17387);
#14047=AXIS2_PLACEMENT_3D('',#32489,#17391,#17392);
#14048=AXIS2_PLACEMENT_3D('',#32495,#17396,#17397);
#14049=AXIS2_PLACEMENT_3D('',#32498,#17400,#17401);
#14050=AXIS2_PLACEMENT_3D('',#32499,#17402,#17403);
#14051=AXIS2_PLACEMENT_3D('',#32500,#17404,#17405);
#14052=AXIS2_PLACEMENT_3D('',#32501,#17406,#17407);
#14053=AXIS2_PLACEMENT_3D('',#32503,#17408,#17409);
#14054=AXIS2_PLACEMENT_3D('',#32504,#17410,#17411);
#14055=AXIS2_PLACEMENT_3D('',#32506,#17412,#17413);
#14056=AXIS2_PLACEMENT_3D('',#32508,#17415,#17416);
#14057=AXIS2_PLACEMENT_3D('',#32510,#17417,#17418);
#14058=AXIS2_PLACEMENT_3D('',#32512,#17420,#17421);
#14059=AXIS2_PLACEMENT_3D('',#32514,#17422,#17423);
#14060=AXIS2_PLACEMENT_3D('',#32516,#17425,#17426);
#14061=AXIS2_PLACEMENT_3D('',#32518,#17427,#17428);
#14062=AXIS2_PLACEMENT_3D('',#32519,#17429,#17430);
#14063=AXIS2_PLACEMENT_3D('',#32521,#17431,#17432);
#14064=AXIS2_PLACEMENT_3D('',#32523,#17434,#17435);
#14065=AXIS2_PLACEMENT_3D('',#32525,#17436,#17437);
#14066=AXIS2_PLACEMENT_3D('',#32527,#17439,#17440);
#14067=AXIS2_PLACEMENT_3D('',#32529,#17441,#17442);
#14068=AXIS2_PLACEMENT_3D('',#32531,#17444,#17445);
#14069=AXIS2_PLACEMENT_3D('',#32532,#17446,#17447);
#14070=AXIS2_PLACEMENT_3D('',#32541,#17452,#17453);
#14071=AXIS2_PLACEMENT_3D('',#32547,#17457,#17458);
#14072=AXIS2_PLACEMENT_3D('',#32553,#17462,#17463);
#14073=AXIS2_PLACEMENT_3D('',#32559,#17467,#17468);
#14074=AXIS2_PLACEMENT_3D('',#32565,#17472,#17473);
#14075=AXIS2_PLACEMENT_3D('',#32568,#17476,#17477);
#14076=AXIS2_PLACEMENT_3D('',#32569,#17478,#17479);
#14077=AXIS2_PLACEMENT_3D('',#32570,#17480,#17481);
#14078=AXIS2_PLACEMENT_3D('',#32571,#17482,#17483);
#14079=AXIS2_PLACEMENT_3D('',#32572,#17484,#17485);
#14080=AXIS2_PLACEMENT_3D('',#32573,#17486,#17487);
#14081=AXIS2_PLACEMENT_3D('',#32574,#17488,#17489);
#14082=AXIS2_PLACEMENT_3D('',#32575,#17490,#17491);
#14083=AXIS2_PLACEMENT_3D('',#32576,#17492,#17493);
#14084=AXIS2_PLACEMENT_3D('',#32577,#17494,#17495);
#14085=AXIS2_PLACEMENT_3D('',#32578,#17496,#17497);
#14086=AXIS2_PLACEMENT_3D('',#32579,#17498,#17499);
#14087=AXIS2_PLACEMENT_3D('',#32580,#17500,#17501);
#14088=AXIS2_PLACEMENT_3D('',#32581,#17502,#17503);
#14089=AXIS2_PLACEMENT_3D('',#32582,#17504,#17505);
#14090=AXIS2_PLACEMENT_3D('',#32583,#17506,#17507);
#14091=AXIS2_PLACEMENT_3D('',#32584,#17508,#17509);
#14092=AXIS2_PLACEMENT_3D('',#32585,#17510,#17511);
#14093=AXIS2_PLACEMENT_3D('',#32586,#17512,#17513);
#14094=AXIS2_PLACEMENT_3D('',#32587,#17514,#17515);
#14095=AXIS2_PLACEMENT_3D('',#32588,#17516,#17517);
#14096=AXIS2_PLACEMENT_3D('',#32589,#17518,#17519);
#14097=AXIS2_PLACEMENT_3D('',#32590,#17520,#17521);
#14098=AXIS2_PLACEMENT_3D('',#32591,#17522,#17523);
#14099=AXIS2_PLACEMENT_3D('',#32592,#17524,#17525);
#14100=AXIS2_PLACEMENT_3D('',#32593,#17526,#17527);
#14101=AXIS2_PLACEMENT_3D('',#32594,#17528,#17529);
#14102=AXIS2_PLACEMENT_3D('',#32595,#17530,#17531);
#14103=AXIS2_PLACEMENT_3D('',#32596,#17532,#17533);
#14104=AXIS2_PLACEMENT_3D('',#32597,#17534,#17535);
#14105=AXIS2_PLACEMENT_3D('',#32598,#17536,#17537);
#14106=AXIS2_PLACEMENT_3D('',#32599,#17538,#17539);
#14107=AXIS2_PLACEMENT_3D('',#32600,#17540,#17541);
#14108=AXIS2_PLACEMENT_3D('',#32601,#17542,#17543);
#14109=AXIS2_PLACEMENT_3D('',#32602,#17544,#17545);
#14110=AXIS2_PLACEMENT_3D('',#32603,#17546,#17547);
#14111=AXIS2_PLACEMENT_3D('',#32604,#17548,#17549);
#14112=AXIS2_PLACEMENT_3D('',#32605,#17550,#17551);
#14113=AXIS2_PLACEMENT_3D('',#32606,#17552,#17553);
#14114=AXIS2_PLACEMENT_3D('',#32607,#17554,#17555);
#14115=AXIS2_PLACEMENT_3D('',#32608,#17556,#17557);
#14116=AXIS2_PLACEMENT_3D('',#32609,#17558,#17559);
#14117=AXIS2_PLACEMENT_3D('',#32610,#17560,#17561);
#14118=AXIS2_PLACEMENT_3D('',#32611,#17562,#17563);
#14119=AXIS2_PLACEMENT_3D('',#32612,#17564,#17565);
#14120=AXIS2_PLACEMENT_3D('',#32613,#17566,#17567);
#14121=AXIS2_PLACEMENT_3D('',#32614,#17568,#17569);
#14122=AXIS2_PLACEMENT_3D('',#32615,#17570,#17571);
#14123=AXIS2_PLACEMENT_3D('',#32616,#17572,#17573);
#14124=AXIS2_PLACEMENT_3D('',#32617,#17574,#17575);
#14125=AXIS2_PLACEMENT_3D('',#32618,#17576,#17577);
#14126=AXIS2_PLACEMENT_3D('',#32619,#17578,#17579);
#14127=AXIS2_PLACEMENT_3D('',#32620,#17580,#17581);
#14128=AXIS2_PLACEMENT_3D('',#32621,#17582,#17583);
#14129=AXIS2_PLACEMENT_3D('',#32622,#17584,#17585);
#14130=AXIS2_PLACEMENT_3D('',#32623,#17586,#17587);
#14131=AXIS2_PLACEMENT_3D('',#32624,#17588,#17589);
#14132=AXIS2_PLACEMENT_3D('',#32625,#17590,#17591);
#14133=AXIS2_PLACEMENT_3D('',#32626,#17592,#17593);
#14134=AXIS2_PLACEMENT_3D('',#32627,#17594,#17595);
#14135=AXIS2_PLACEMENT_3D('',#32628,#17596,#17597);
#14136=AXIS2_PLACEMENT_3D('',#32629,#17598,#17599);
#14137=AXIS2_PLACEMENT_3D('',#32630,#17600,#17601);
#14138=AXIS2_PLACEMENT_3D('',#32631,#17602,#17603);
#14139=AXIS2_PLACEMENT_3D('',#32632,#17604,#17605);
#14140=AXIS2_PLACEMENT_3D('',#32633,#17606,#17607);
#14141=AXIS2_PLACEMENT_3D('',#32634,#17608,#17609);
#14142=AXIS2_PLACEMENT_3D('',#32635,#17610,#17611);
#14143=AXIS2_PLACEMENT_3D('',#32637,#17612,#17613);
#14144=AXIS2_PLACEMENT_3D('',#32640,#17615,#17616);
#14145=AXIS2_PLACEMENT_3D('',#32641,#17617,#17618);
#14146=AXIS2_PLACEMENT_3D('',#32643,#17619,#17620);
#14147=AXIS2_PLACEMENT_3D('',#32646,#17622,#17623);
#14148=AXIS2_PLACEMENT_3D('',#32647,#17624,#17625);
#14149=AXIS2_PLACEMENT_3D('',#32648,#17626,#17627);
#14150=AXIS2_PLACEMENT_3D('',#32649,#17628,#17629);
#14151=AXIS2_PLACEMENT_3D('',#32650,#17630,#17631);
#14152=AXIS2_PLACEMENT_3D('',#32651,#17632,#17633);
#14153=AXIS2_PLACEMENT_3D('',#32652,#17634,#17635);
#14154=AXIS2_PLACEMENT_3D('',#32653,#17636,#17637);
#14155=DIRECTION('axis',(0.,0.,1.));
#14156=DIRECTION('refdir',(1.,0.,0.));
#14157=DIRECTION('axis',(0.,0.,1.));
#14158=DIRECTION('refdir',(1.,0.,0.));
#14159=DIRECTION('axis',(0.,0.,1.));
#14160=DIRECTION('refdir',(1.,0.,0.));
#14161=DIRECTION('center_axis',(0.,0.,1.));
#14162=DIRECTION('ref_axis',(1.,0.,0.));
#14163=DIRECTION('center_axis',(0.,0.,1.));
#14164=DIRECTION('ref_axis',(1.,0.,0.));
#14165=DIRECTION('',(0.,0.,1.));
#14166=DIRECTION('center_axis',(0.,0.,-1.));
#14167=DIRECTION('ref_axis',(1.,0.,0.));
#14168=DIRECTION('center_axis',(0.,0.,1.));
#14169=DIRECTION('ref_axis',(1.,0.,0.));
#14170=DIRECTION('center_axis',(0.,0.,1.));
#14171=DIRECTION('ref_axis',(1.,0.,0.));
#14172=DIRECTION('',(0.,0.,1.));
#14173=DIRECTION('center_axis',(0.,0.,-1.));
#14174=DIRECTION('ref_axis',(1.,0.,0.));
#14175=DIRECTION('center_axis',(0.,0.,1.));
#14176=DIRECTION('ref_axis',(1.,0.,0.));
#14177=DIRECTION('center_axis',(0.,0.,1.));
#14178=DIRECTION('ref_axis',(1.,0.,0.));
#14179=DIRECTION('',(0.,0.,1.));
#14180=DIRECTION('center_axis',(0.,0.,-1.));
#14181=DIRECTION('ref_axis',(1.,0.,0.));
#14182=DIRECTION('center_axis',(0.,0.,1.));
#14183=DIRECTION('ref_axis',(1.,0.,0.));
#14184=DIRECTION('center_axis',(0.,0.,1.));
#14185=DIRECTION('ref_axis',(1.,0.,0.));
#14186=DIRECTION('',(0.,0.,1.));
#14187=DIRECTION('center_axis',(0.,0.,-1.));
#14188=DIRECTION('ref_axis',(1.,0.,0.));
#14189=DIRECTION('center_axis',(0.,0.,1.));
#14190=DIRECTION('ref_axis',(1.,0.,0.));
#14191=DIRECTION('center_axis',(0.,0.,1.));
#14192=DIRECTION('ref_axis',(1.,0.,0.));
#14193=DIRECTION('',(0.,0.,1.));
#14194=DIRECTION('center_axis',(0.,0.,-1.));
#14195=DIRECTION('ref_axis',(1.,0.,0.));
#14196=DIRECTION('center_axis',(0.,0.,1.));
#14197=DIRECTION('ref_axis',(1.,0.,0.));
#14198=DIRECTION('center_axis',(0.,0.,1.));
#14199=DIRECTION('ref_axis',(1.,0.,0.));
#14200=DIRECTION('',(0.,0.,1.));
#14201=DIRECTION('center_axis',(0.,0.,-1.));
#14202=DIRECTION('ref_axis',(1.,0.,0.));
#14203=DIRECTION('center_axis',(0.,0.,1.));
#14204=DIRECTION('ref_axis',(1.,0.,0.));
#14205=DIRECTION('center_axis',(0.,0.,1.));
#14206=DIRECTION('ref_axis',(1.,0.,0.));
#14207=DIRECTION('',(0.,0.,1.));
#14208=DIRECTION('center_axis',(0.,0.,-1.));
#14209=DIRECTION('ref_axis',(1.,0.,0.));
#14210=DIRECTION('center_axis',(0.,0.,1.));
#14211=DIRECTION('ref_axis',(1.,0.,0.));
#14212=DIRECTION('center_axis',(0.,0.,1.));
#14213=DIRECTION('ref_axis',(1.,0.,0.));
#14214=DIRECTION('',(0.,0.,1.));
#14215=DIRECTION('center_axis',(0.,0.,-1.));
#14216=DIRECTION('ref_axis',(1.,0.,0.));
#14217=DIRECTION('center_axis',(0.,0.,1.));
#14218=DIRECTION('ref_axis',(1.,0.,0.));
#14219=DIRECTION('center_axis',(0.,0.,1.));
#14220=DIRECTION('ref_axis',(1.,0.,0.));
#14221=DIRECTION('',(0.,0.,1.));
#14222=DIRECTION('center_axis',(0.,0.,-1.));
#14223=DIRECTION('ref_axis',(1.,0.,0.));
#14224=DIRECTION('center_axis',(0.,0.,1.));
#14225=DIRECTION('ref_axis',(1.,0.,0.));
#14226=DIRECTION('center_axis',(0.,0.,1.));
#14227=DIRECTION('ref_axis',(1.,0.,0.));
#14228=DIRECTION('',(0.,0.,1.));
#14229=DIRECTION('center_axis',(0.,0.,-1.));
#14230=DIRECTION('ref_axis',(1.,0.,0.));
#14231=DIRECTION('center_axis',(0.,1.,0.));
#14232=DIRECTION('ref_axis',(-1.,0.,0.));
#14233=DIRECTION('',(-1.,0.,0.));
#14234=DIRECTION('',(0.,0.,1.));
#14235=DIRECTION('',(-1.,0.,0.));
#14236=DIRECTION('',(0.,0.,1.));
#14237=DIRECTION('center_axis',(1.,0.,0.));
#14238=DIRECTION('ref_axis',(0.,1.,0.));
#14239=DIRECTION('',(0.,1.,0.));
#14240=DIRECTION('',(0.,1.,0.));
#14241=DIRECTION('',(0.,0.,1.));
#14242=DIRECTION('center_axis',(0.,-1.,0.));
#14243=DIRECTION('ref_axis',(1.,0.,0.));
#14244=DIRECTION('',(1.,0.,0.));
#14245=DIRECTION('',(1.,0.,0.));
#14246=DIRECTION('',(0.,0.,1.));
#14247=DIRECTION('center_axis',(-1.,0.,0.));
#14248=DIRECTION('ref_axis',(0.,-1.,0.));
#14249=DIRECTION('',(0.,-1.,0.));
#14250=DIRECTION('',(0.,-1.,0.));
#14251=DIRECTION('center_axis',(0.,0.,1.));
#14252=DIRECTION('ref_axis',(1.,0.,0.));
#14253=DIRECTION('center_axis',(0.,0.,1.));
#14254=DIRECTION('ref_axis',(1.,0.,0.));
#14255=DIRECTION('axis',(0.,0.,1.));
#14256=DIRECTION('refdir',(1.,0.,0.));
#14257=DIRECTION('center_axis',(0.,1.,0.));
#14258=DIRECTION('ref_axis',(-1.,0.,0.));
#14259=DIRECTION('',(-1.,0.,0.));
#14260=DIRECTION('',(0.,0.,1.));
#14261=DIRECTION('',(-1.,0.,0.));
#14262=DIRECTION('',(0.,0.,1.));
#14263=DIRECTION('center_axis',(1.,0.,0.));
#14264=DIRECTION('ref_axis',(0.,1.,0.));
#14265=DIRECTION('',(0.,1.,0.));
#14266=DIRECTION('',(0.,1.,0.));
#14267=DIRECTION('',(0.,0.,1.));
#14268=DIRECTION('center_axis',(0.,-1.,0.));
#14269=DIRECTION('ref_axis',(1.,0.,0.));
#14270=DIRECTION('',(1.,0.,0.));
#14271=DIRECTION('',(1.,0.,0.));
#14272=DIRECTION('',(0.,0.,1.));
#14273=DIRECTION('center_axis',(-1.,0.,0.));
#14274=DIRECTION('ref_axis',(0.,-1.,0.));
#14275=DIRECTION('',(0.,-1.,0.));
#14276=DIRECTION('',(0.,-1.,0.));
#14277=DIRECTION('center_axis',(0.,0.,1.));
#14278=DIRECTION('ref_axis',(1.,0.,0.));
#14279=DIRECTION('center_axis',(0.,0.,1.));
#14280=DIRECTION('ref_axis',(1.,0.,0.));
#14281=DIRECTION('axis',(0.,0.,1.));
#14282=DIRECTION('refdir',(1.,0.,0.));
#14283=DIRECTION('center_axis',(0.,1.,0.));
#14284=DIRECTION('ref_axis',(-1.,0.,0.));
#14285=DIRECTION('',(-1.,0.,0.));
#14286=DIRECTION('',(0.,0.,1.));
#14287=DIRECTION('',(-1.,0.,0.));
#14288=DIRECTION('',(0.,0.,1.));
#14289=DIRECTION('center_axis',(1.,0.,0.));
#14290=DIRECTION('ref_axis',(0.,1.,0.));
#14291=DIRECTION('',(0.,1.,0.));
#14292=DIRECTION('',(0.,1.,0.));
#14293=DIRECTION('',(0.,0.,1.));
#14294=DIRECTION('center_axis',(0.,-1.,0.));
#14295=DIRECTION('ref_axis',(1.,0.,0.));
#14296=DIRECTION('',(1.,0.,0.));
#14297=DIRECTION('',(1.,0.,0.));
#14298=DIRECTION('',(0.,0.,1.));
#14299=DIRECTION('center_axis',(-1.,0.,0.));
#14300=DIRECTION('ref_axis',(0.,-1.,0.));
#14301=DIRECTION('',(0.,-1.,0.));
#14302=DIRECTION('',(0.,-1.,0.));
#14303=DIRECTION('center_axis',(0.,0.,1.));
#14304=DIRECTION('ref_axis',(1.,0.,0.));
#14305=DIRECTION('center_axis',(0.,0.,1.));
#14306=DIRECTION('ref_axis',(1.,0.,0.));
#14307=DIRECTION('axis',(0.,0.,1.));
#14308=DIRECTION('refdir',(1.,0.,0.));
#14309=DIRECTION('center_axis',(0.,0.,1.));
#14310=DIRECTION('ref_axis',(1.,0.,0.));
#14311=DIRECTION('center_axis',(0.,0.,1.));
#14312=DIRECTION('ref_axis',(1.,0.,0.));
#14313=DIRECTION('',(0.,0.,1.));
#14314=DIRECTION('center_axis',(0.,0.,-1.));
#14315=DIRECTION('ref_axis',(1.,0.,0.));
#14316=DIRECTION('center_axis',(0.,0.,1.));
#14317=DIRECTION('ref_axis',(1.,0.,0.));
#14318=DIRECTION('center_axis',(0.,0.,1.));
#14319=DIRECTION('ref_axis',(1.,0.,0.));
#14320=DIRECTION('center_axis',(0.,0.,1.));
#14321=DIRECTION('ref_axis',(1.,0.,0.));
#14322=DIRECTION('',(0.,0.,1.));
#14323=DIRECTION('center_axis',(0.,0.,-1.));
#14324=DIRECTION('ref_axis',(1.,0.,0.));
#14325=DIRECTION('center_axis',(0.,0.,1.));
#14326=DIRECTION('ref_axis',(1.,0.,0.));
#14327=DIRECTION('center_axis',(0.,1.,0.));
#14328=DIRECTION('ref_axis',(-1.,0.,0.));
#14329=DIRECTION('',(0.,0.,1.));
#14330=DIRECTION('',(-1.,0.,0.));
#14331=DIRECTION('',(0.,0.,-1.));
#14332=DIRECTION('',(1.,0.,0.));
#14333=DIRECTION('center_axis',(0.,-1.,0.));
#14334=DIRECTION('ref_axis',(1.,0.,0.));
#14335=DIRECTION('',(0.,0.,-1.));
#14336=DIRECTION('',(-1.,0.,0.));
#14337=DIRECTION('',(0.,0.,1.));
#14338=DIRECTION('',(1.,0.,0.));
#14339=DIRECTION('center_axis',(0.,0.,1.));
#14340=DIRECTION('ref_axis',(1.,0.,0.));
#14341=DIRECTION('center_axis',(0.,0.,1.));
#14342=DIRECTION('ref_axis',(1.,0.,0.));
#14343=DIRECTION('',(-1.,0.,0.));
#14344=DIRECTION('',(0.,1.,0.));
#14345=DIRECTION('',(1.,0.,0.));
#14346=DIRECTION('center_axis',(0.,0.,1.));
#14347=DIRECTION('ref_axis',(1.,0.,0.));
#14348=DIRECTION('center_axis',(0.,0.,1.));
#14349=DIRECTION('ref_axis',(1.,0.,0.));
#14350=DIRECTION('center_axis',(0.,0.,1.));
#14351=DIRECTION('ref_axis',(1.,0.,0.));
#14352=DIRECTION('center_axis',(0.,0.,-1.));
#14353=DIRECTION('ref_axis',(1.,0.,0.));
#14354=DIRECTION('center_axis',(0.,0.,1.));
#14355=DIRECTION('ref_axis',(1.,0.,0.));
#14356=DIRECTION('',(0.,0.,1.));
#14357=DIRECTION('center_axis',(0.,0.,1.));
#14358=DIRECTION('ref_axis',(1.,0.,0.));
#14359=DIRECTION('center_axis',(0.,0.,1.));
#14360=DIRECTION('ref_axis',(1.,0.,0.));
#14361=DIRECTION('center_axis',(0.,0.,1.));
#14362=DIRECTION('ref_axis',(1.,0.,0.));
#14363=DIRECTION('',(0.,0.,1.));
#14364=DIRECTION('center_axis',(0.,0.,1.));
#14365=DIRECTION('ref_axis',(1.,0.,0.));
#14366=DIRECTION('',(1.,0.,0.));
#14367=DIRECTION('',(0.,-1.,0.));
#14368=DIRECTION('',(-1.,0.,0.));
#14369=DIRECTION('center_axis',(0.,-1.,0.));
#14370=DIRECTION('ref_axis',(1.,0.,0.));
#14371=DIRECTION('',(0.,0.,-1.));
#14372=DIRECTION('center_axis',(0.,1.,0.));
#14373=DIRECTION('ref_axis',(-1.,0.,0.));
#14374=DIRECTION('',(0.,0.,1.));
#14375=DIRECTION('center_axis',(0.,0.,1.));
#14376=DIRECTION('ref_axis',(1.,0.,0.));
#14377=DIRECTION('center_axis',(0.,0.,1.));
#14378=DIRECTION('ref_axis',(1.,0.,0.));
#14379=DIRECTION('',(0.,0.,1.));
#14380=DIRECTION('center_axis',(0.,0.,-1.));
#14381=DIRECTION('ref_axis',(1.,0.,0.));
#14382=DIRECTION('center_axis',(0.,0.,1.));
#14383=DIRECTION('ref_axis',(1.,0.,0.));
#14384=DIRECTION('center_axis',(0.,0.,1.));
#14385=DIRECTION('ref_axis',(1.,0.,0.));
#14386=DIRECTION('center_axis',(0.,0.,1.));
#14387=DIRECTION('ref_axis',(1.,0.,0.));
#14388=DIRECTION('',(0.,0.,1.));
#14389=DIRECTION('center_axis',(0.,0.,-1.));
#14390=DIRECTION('ref_axis',(1.,0.,0.));
#14391=DIRECTION('center_axis',(0.,0.,1.));
#14392=DIRECTION('ref_axis',(1.,0.,0.));
#14393=DIRECTION('center_axis',(0.,1.,0.));
#14394=DIRECTION('ref_axis',(-1.,0.,0.));
#14395=DIRECTION('',(0.,0.,1.));
#14396=DIRECTION('',(-1.,0.,0.));
#14397=DIRECTION('',(0.,0.,-1.));
#14398=DIRECTION('',(1.,0.,0.));
#14399=DIRECTION('center_axis',(0.,-1.,0.));
#14400=DIRECTION('ref_axis',(1.,0.,0.));
#14401=DIRECTION('',(0.,0.,-1.));
#14402=DIRECTION('',(-1.,0.,0.));
#14403=DIRECTION('',(0.,0.,1.));
#14404=DIRECTION('',(1.,0.,0.));
#14405=DIRECTION('center_axis',(0.,0.,1.));
#14406=DIRECTION('ref_axis',(1.,0.,0.));
#14407=DIRECTION('center_axis',(0.,0.,1.));
#14408=DIRECTION('ref_axis',(1.,0.,0.));
#14409=DIRECTION('',(-1.,0.,0.));
#14410=DIRECTION('',(0.,1.,0.));
#14411=DIRECTION('',(1.,0.,0.));
#14412=DIRECTION('center_axis',(0.,0.,1.));
#14413=DIRECTION('ref_axis',(1.,0.,0.));
#14414=DIRECTION('center_axis',(0.,0.,1.));
#14415=DIRECTION('ref_axis',(1.,0.,0.));
#14416=DIRECTION('center_axis',(0.,0.,1.));
#14417=DIRECTION('ref_axis',(1.,0.,0.));
#14418=DIRECTION('center_axis',(0.,0.,-1.));
#14419=DIRECTION('ref_axis',(1.,0.,0.));
#14420=DIRECTION('center_axis',(0.,0.,1.));
#14421=DIRECTION('ref_axis',(1.,0.,0.));
#14422=DIRECTION('',(0.,0.,1.));
#14423=DIRECTION('center_axis',(0.,0.,1.));
#14424=DIRECTION('ref_axis',(1.,0.,0.));
#14425=DIRECTION('center_axis',(0.,0.,1.));
#14426=DIRECTION('ref_axis',(1.,0.,0.));
#14427=DIRECTION('center_axis',(0.,0.,1.));
#14428=DIRECTION('ref_axis',(1.,0.,0.));
#14429=DIRECTION('',(0.,0.,1.));
#14430=DIRECTION('center_axis',(0.,0.,1.));
#14431=DIRECTION('ref_axis',(1.,0.,0.));
#14432=DIRECTION('',(1.,0.,0.));
#14433=DIRECTION('',(0.,-1.,0.));
#14434=DIRECTION('',(-1.,0.,0.));
#14435=DIRECTION('center_axis',(0.,-1.,0.));
#14436=DIRECTION('ref_axis',(1.,0.,0.));
#14437=DIRECTION('',(0.,0.,-1.));
#14438=DIRECTION('center_axis',(0.,1.,0.));
#14439=DIRECTION('ref_axis',(-1.,0.,0.));
#14440=DIRECTION('',(0.,0.,1.));
#14441=DIRECTION('center_axis',(0.,0.,1.));
#14442=DIRECTION('ref_axis',(1.,0.,0.));
#14443=DIRECTION('center_axis',(0.,0.,1.));
#14444=DIRECTION('ref_axis',(1.,0.,0.));
#14445=DIRECTION('',(0.,0.,1.));
#14446=DIRECTION('center_axis',(0.,0.,-1.));
#14447=DIRECTION('ref_axis',(1.,0.,0.));
#14448=DIRECTION('center_axis',(0.,0.,1.));
#14449=DIRECTION('ref_axis',(1.,0.,0.));
#14450=DIRECTION('center_axis',(0.,0.,1.));
#14451=DIRECTION('ref_axis',(1.,0.,0.));
#14452=DIRECTION('',(0.,0.,1.));
#14453=DIRECTION('center_axis',(0.,0.,-1.));
#14454=DIRECTION('ref_axis',(1.,0.,0.));
#14455=DIRECTION('center_axis',(0.,0.,1.));
#14456=DIRECTION('ref_axis',(1.,0.,0.));
#14457=DIRECTION('center_axis',(0.,0.,1.));
#14458=DIRECTION('ref_axis',(1.,0.,0.));
#14459=DIRECTION('',(0.,0.,1.));
#14460=DIRECTION('center_axis',(0.,0.,-1.));
#14461=DIRECTION('ref_axis',(1.,0.,0.));
#14462=DIRECTION('center_axis',(0.,0.,1.));
#14463=DIRECTION('ref_axis',(1.,0.,0.));
#14464=DIRECTION('center_axis',(0.,0.,1.));
#14465=DIRECTION('ref_axis',(1.,0.,0.));
#14466=DIRECTION('',(0.,0.,1.));
#14467=DIRECTION('center_axis',(0.,0.,-1.));
#14468=DIRECTION('ref_axis',(1.,0.,0.));
#14469=DIRECTION('center_axis',(0.,0.,1.));
#14470=DIRECTION('ref_axis',(1.,0.,0.));
#14471=DIRECTION('',(0.,-1.,0.));
#14472=DIRECTION('',(1.,0.,0.));
#14473=DIRECTION('',(0.,1.,0.));
#14474=DIRECTION('',(-1.,0.,0.));
#14475=DIRECTION('',(-1.,0.,0.));
#14476=DIRECTION('',(0.,1.,0.));
#14477=DIRECTION('',(1.,0.,0.));
#14478=DIRECTION('',(0.,-1.,0.));
#14479=DIRECTION('center_axis',(0.,1.,0.));
#14480=DIRECTION('ref_axis',(-1.,0.,0.));
#14481=DIRECTION('',(-1.,0.,0.));
#14482=DIRECTION('',(0.,0.,1.));
#14483=DIRECTION('',(0.,0.,1.));
#14484=DIRECTION('center_axis',(1.,0.,0.));
#14485=DIRECTION('ref_axis',(0.,1.,0.));
#14486=DIRECTION('',(0.,1.,0.));
#14487=DIRECTION('',(0.,0.,1.));
#14488=DIRECTION('center_axis',(0.,-1.,0.));
#14489=DIRECTION('ref_axis',(1.,0.,0.));
#14490=DIRECTION('',(1.,0.,0.));
#14491=DIRECTION('',(0.,0.,1.));
#14492=DIRECTION('center_axis',(-1.,0.,0.));
#14493=DIRECTION('ref_axis',(0.,-1.,0.));
#14494=DIRECTION('',(0.,-1.,0.));
#14495=DIRECTION('center_axis',(0.,-1.,0.));
#14496=DIRECTION('ref_axis',(1.,0.,0.));
#14497=DIRECTION('',(0.,0.,1.));
#14498=DIRECTION('',(1.,0.,0.));
#14499=DIRECTION('',(0.,0.,1.));
#14500=DIRECTION('center_axis',(1.,0.,0.));
#14501=DIRECTION('ref_axis',(0.,1.,0.));
#14502=DIRECTION('',(0.,0.,1.));
#14503=DIRECTION('',(0.,1.,0.));
#14504=DIRECTION('center_axis',(0.,1.,0.));
#14505=DIRECTION('ref_axis',(-1.,0.,0.));
#14506=DIRECTION('',(0.,0.,1.));
#14507=DIRECTION('',(-1.,0.,0.));
#14508=DIRECTION('center_axis',(-1.,0.,0.));
#14509=DIRECTION('ref_axis',(0.,-1.,0.));
#14510=DIRECTION('',(0.,-1.,0.));
#14511=DIRECTION('center_axis',(0.,0.,1.));
#14512=DIRECTION('ref_axis',(1.,0.,0.));
#14513=DIRECTION('center_axis',(0.,0.,1.));
#14514=DIRECTION('ref_axis',(1.,0.,0.));
#14515=DIRECTION('axis',(0.,0.,1.));
#14516=DIRECTION('refdir',(1.,0.,0.));
#14517=DIRECTION('center_axis',(1.,0.,0.));
#14518=DIRECTION('ref_axis',(0.,1.,0.));
#14519=DIRECTION('',(0.,1.,0.));
#14520=DIRECTION('',(0.,0.,1.));
#14521=DIRECTION('',(0.,-1.,0.));
#14522=DIRECTION('',(0.,0.,1.));
#14523=DIRECTION('center_axis',(1.,0.,0.));
#14524=DIRECTION('ref_axis',(0.,1.,0.));
#14525=DIRECTION('',(0.,-1.,0.));
#14526=DIRECTION('',(0.,0.,1.));
#14527=DIRECTION('',(0.,1.,0.));
#14528=DIRECTION('',(0.,0.,-1.));
#14529=DIRECTION('center_axis',(0.,1.,0.));
#14530=DIRECTION('ref_axis',(-1.,0.,0.));
#14531=DIRECTION('',(1.,0.,0.));
#14532=DIRECTION('',(0.,0.,1.));
#14533=DIRECTION('',(-1.,0.,0.));
#14534=DIRECTION('',(0.,0.,1.));
#14535=DIRECTION('',(-1.,0.,0.));
#14536=DIRECTION('center_axis',(0.,-1.,0.));
#14537=DIRECTION('ref_axis',(1.,0.,0.));
#14538=DIRECTION('',(1.,0.,0.));
#14539=DIRECTION('',(0.,0.,-1.));
#14540=DIRECTION('',(1.,0.,0.));
#14541=DIRECTION('',(0.,0.,-1.));
#14542=DIRECTION('',(-1.,0.,0.));
#14543=DIRECTION('center_axis',(0.,0.,1.));
#14544=DIRECTION('ref_axis',(1.,0.,0.));
#14545=DIRECTION('center_axis',(0.,0.,1.));
#14546=DIRECTION('ref_axis',(1.,0.,0.));
#14547=DIRECTION('center_axis',(0.,0.,-1.));
#14548=DIRECTION('ref_axis',(1.,0.,0.));
#14549=DIRECTION('center_axis',(0.,0.,1.));
#14550=DIRECTION('ref_axis',(1.,0.,0.));
#14551=DIRECTION('center_axis',(0.,0.,-1.));
#14552=DIRECTION('ref_axis',(1.,0.,0.));
#14553=DIRECTION('center_axis',(0.,0.,1.));
#14554=DIRECTION('ref_axis',(1.,0.,0.));
#14555=DIRECTION('center_axis',(0.,0.,1.));
#14556=DIRECTION('ref_axis',(1.,0.,0.));
#14557=DIRECTION('center_axis',(0.,0.,1.));
#14558=DIRECTION('ref_axis',(1.,0.,0.));
#14559=DIRECTION('center_axis',(0.,0.,1.));
#14560=DIRECTION('ref_axis',(1.,0.,0.));
#14561=DIRECTION('center_axis',(0.,0.,1.));
#14562=DIRECTION('ref_axis',(1.,0.,0.));
#14563=DIRECTION('center_axis',(0.,0.,1.));
#14564=DIRECTION('ref_axis',(1.,0.,0.));
#14565=DIRECTION('center_axis',(0.,0.,1.));
#14566=DIRECTION('ref_axis',(1.,0.,0.));
#14567=DIRECTION('axis',(0.,0.,1.));
#14568=DIRECTION('refdir',(1.,0.,0.));
#14569=DIRECTION('center_axis',(0.,0.,1.));
#14570=DIRECTION('ref_axis',(1.,0.,0.));
#14571=DIRECTION('center_axis',(0.,0.,1.));
#14572=DIRECTION('ref_axis',(1.,0.,0.));
#14573=DIRECTION('',(0.,0.,1.));
#14574=DIRECTION('center_axis',(0.,0.,-1.));
#14575=DIRECTION('ref_axis',(1.,0.,0.));
#14576=DIRECTION('center_axis',(0.,0.,1.));
#14577=DIRECTION('ref_axis',(1.,0.,0.));
#14578=DIRECTION('center_axis',(0.,0.,1.));
#14579=DIRECTION('ref_axis',(1.,0.,0.));
#14580=DIRECTION('',(0.,0.,1.));
#14581=DIRECTION('center_axis',(0.,0.,-1.));
#14582=DIRECTION('ref_axis',(1.,0.,0.));
#14583=DIRECTION('center_axis',(0.,1.,0.));
#14584=DIRECTION('ref_axis',(-1.,0.,0.));
#14585=DIRECTION('',(-1.,0.,0.));
#14586=DIRECTION('',(0.,0.,1.));
#14587=DIRECTION('',(1.,0.,0.));
#14588=DIRECTION('',(0.,0.,1.));
#14589=DIRECTION('center_axis',(0.,-1.,0.));
#14590=DIRECTION('ref_axis',(1.,0.,0.));
#14591=DIRECTION('',(-1.,0.,0.));
#14592=DIRECTION('',(0.,0.,1.));
#14593=DIRECTION('',(1.,0.,0.));
#14594=DIRECTION('',(0.,0.,-1.));
#14595=DIRECTION('center_axis',(1.,0.,0.));
#14596=DIRECTION('ref_axis',(0.,1.,0.));
#14597=DIRECTION('',(0.,-1.,0.));
#14598=DIRECTION('',(0.,0.,1.));
#14599=DIRECTION('',(0.,1.,0.));
#14600=DIRECTION('center_axis',(1.,0.,0.));
#14601=DIRECTION('ref_axis',(0.,1.,0.));
#14602=DIRECTION('',(0.,1.,0.));
#14603=DIRECTION('',(0.,0.,-1.));
#14604=DIRECTION('',(0.,-1.,0.));
#14605=DIRECTION('center_axis',(-1.,0.,0.));
#14606=DIRECTION('ref_axis',(0.,-1.,0.));
#14607=DIRECTION('',(0.,-1.,0.));
#14608=DIRECTION('',(0.,0.,1.));
#14609=DIRECTION('',(0.,-1.,0.));
#14610=DIRECTION('center_axis',(-1.,0.,0.));
#14611=DIRECTION('ref_axis',(0.,-1.,0.));
#14612=DIRECTION('',(0.,-1.,0.));
#14613=DIRECTION('',(0.,0.,1.));
#14614=DIRECTION('',(0.,-1.,0.));
#14615=DIRECTION('center_axis',(0.,0.,1.));
#14616=DIRECTION('ref_axis',(1.,0.,0.));
#14617=DIRECTION('center_axis',(0.,0.,-1.));
#14618=DIRECTION('ref_axis',(1.,0.,0.));
#14619=DIRECTION('',(1.,0.,0.));
#14620=DIRECTION('',(0.,1.,0.));
#14621=DIRECTION('',(-1.,0.,0.));
#14622=DIRECTION('center_axis',(0.,0.,1.));
#14623=DIRECTION('ref_axis',(1.,0.,0.));
#14624=DIRECTION('center_axis',(0.,0.,1.));
#14625=DIRECTION('ref_axis',(1.,0.,0.));
#14626=DIRECTION('center_axis',(0.,1.,0.));
#14627=DIRECTION('ref_axis',(-1.,0.,0.));
#14628=DIRECTION('',(-1.,0.,0.));
#14629=DIRECTION('',(0.,0.,1.));
#14630=DIRECTION('center_axis',(1.,0.,0.));
#14631=DIRECTION('ref_axis',(0.,1.,0.));
#14632=DIRECTION('',(0.,1.,0.));
#14633=DIRECTION('',(0.,0.,1.));
#14634=DIRECTION('center_axis',(0.,-1.,0.));
#14635=DIRECTION('ref_axis',(1.,0.,0.));
#14636=DIRECTION('',(1.,0.,0.));
#14637=DIRECTION('center_axis',(0.,0.,1.));
#14638=DIRECTION('ref_axis',(1.,0.,0.));
#14639=DIRECTION('axis',(0.,0.,1.));
#14640=DIRECTION('refdir',(1.,0.,0.));
#14641=DIRECTION('center_axis',(1.,0.,0.));
#14642=DIRECTION('ref_axis',(0.,1.,0.));
#14643=DIRECTION('',(0.,1.,0.));
#14644=DIRECTION('',(0.,0.,1.));
#14645=DIRECTION('',(0.,-1.,0.));
#14646=DIRECTION('',(0.,0.,1.));
#14647=DIRECTION('center_axis',(1.,0.,0.));
#14648=DIRECTION('ref_axis',(0.,1.,0.));
#14649=DIRECTION('',(0.,-1.,0.));
#14650=DIRECTION('',(0.,0.,1.));
#14651=DIRECTION('',(0.,1.,0.));
#14652=DIRECTION('',(0.,0.,-1.));
#14653=DIRECTION('center_axis',(0.,1.,0.));
#14654=DIRECTION('ref_axis',(-1.,0.,0.));
#14655=DIRECTION('',(1.,0.,0.));
#14656=DIRECTION('',(0.,0.,1.));
#14657=DIRECTION('',(-1.,0.,0.));
#14658=DIRECTION('',(0.,0.,1.));
#14659=DIRECTION('',(-1.,0.,0.));
#14660=DIRECTION('center_axis',(0.,-1.,0.));
#14661=DIRECTION('ref_axis',(1.,0.,0.));
#14662=DIRECTION('',(1.,0.,0.));
#14663=DIRECTION('',(0.,0.,-1.));
#14664=DIRECTION('',(1.,0.,0.));
#14665=DIRECTION('',(0.,0.,-1.));
#14666=DIRECTION('',(-1.,0.,0.));
#14667=DIRECTION('center_axis',(0.,0.,1.));
#14668=DIRECTION('ref_axis',(1.,0.,0.));
#14669=DIRECTION('center_axis',(0.,0.,1.));
#14670=DIRECTION('ref_axis',(1.,0.,0.));
#14671=DIRECTION('center_axis',(0.,0.,-1.));
#14672=DIRECTION('ref_axis',(1.,0.,0.));
#14673=DIRECTION('center_axis',(0.,0.,1.));
#14674=DIRECTION('ref_axis',(1.,0.,0.));
#14675=DIRECTION('center_axis',(0.,0.,-1.));
#14676=DIRECTION('ref_axis',(1.,0.,0.));
#14677=DIRECTION('center_axis',(0.,0.,1.));
#14678=DIRECTION('ref_axis',(1.,0.,0.));
#14679=DIRECTION('center_axis',(0.,0.,1.));
#14680=DIRECTION('ref_axis',(1.,0.,0.));
#14681=DIRECTION('center_axis',(0.,0.,1.));
#14682=DIRECTION('ref_axis',(1.,0.,0.));
#14683=DIRECTION('center_axis',(0.,0.,1.));
#14684=DIRECTION('ref_axis',(1.,0.,0.));
#14685=DIRECTION('center_axis',(0.,0.,1.));
#14686=DIRECTION('ref_axis',(1.,0.,0.));
#14687=DIRECTION('center_axis',(0.,0.,1.));
#14688=DIRECTION('ref_axis',(1.,0.,0.));
#14689=DIRECTION('center_axis',(0.,0.,1.));
#14690=DIRECTION('ref_axis',(1.,0.,0.));
#14691=DIRECTION('axis',(0.,0.,1.));
#14692=DIRECTION('refdir',(1.,0.,0.));
#14693=DIRECTION('center_axis',(0.,0.,1.));
#14694=DIRECTION('ref_axis',(1.,0.,0.));
#14695=DIRECTION('center_axis',(0.,0.,1.));
#14696=DIRECTION('ref_axis',(1.,0.,0.));
#14697=DIRECTION('',(0.,0.,1.));
#14698=DIRECTION('center_axis',(0.,0.,-1.));
#14699=DIRECTION('ref_axis',(1.,0.,0.));
#14700=DIRECTION('center_axis',(0.,0.,1.));
#14701=DIRECTION('ref_axis',(1.,0.,0.));
#14702=DIRECTION('center_axis',(0.,0.,1.));
#14703=DIRECTION('ref_axis',(1.,0.,0.));
#14704=DIRECTION('',(0.,0.,1.));
#14705=DIRECTION('center_axis',(0.,0.,-1.));
#14706=DIRECTION('ref_axis',(1.,0.,0.));
#14707=DIRECTION('center_axis',(0.,1.,0.));
#14708=DIRECTION('ref_axis',(-1.,0.,0.));
#14709=DIRECTION('',(-1.,0.,0.));
#14710=DIRECTION('',(0.,0.,1.));
#14711=DIRECTION('',(1.,0.,0.));
#14712=DIRECTION('',(0.,0.,1.));
#14713=DIRECTION('center_axis',(0.,-1.,0.));
#14714=DIRECTION('ref_axis',(1.,0.,0.));
#14715=DIRECTION('',(-1.,0.,0.));
#14716=DIRECTION('',(0.,0.,1.));
#14717=DIRECTION('',(1.,0.,0.));
#14718=DIRECTION('',(0.,0.,-1.));
#14719=DIRECTION('center_axis',(1.,0.,0.));
#14720=DIRECTION('ref_axis',(0.,1.,0.));
#14721=DIRECTION('',(0.,-1.,0.));
#14722=DIRECTION('',(0.,0.,1.));
#14723=DIRECTION('',(0.,1.,0.));
#14724=DIRECTION('center_axis',(1.,0.,0.));
#14725=DIRECTION('ref_axis',(0.,1.,0.));
#14726=DIRECTION('',(0.,1.,0.));
#14727=DIRECTION('',(0.,0.,-1.));
#14728=DIRECTION('',(0.,-1.,0.));
#14729=DIRECTION('center_axis',(-1.,0.,0.));
#14730=DIRECTION('ref_axis',(0.,-1.,0.));
#14731=DIRECTION('',(0.,-1.,0.));
#14732=DIRECTION('',(0.,0.,1.));
#14733=DIRECTION('',(0.,-1.,0.));
#14734=DIRECTION('center_axis',(-1.,0.,0.));
#14735=DIRECTION('ref_axis',(0.,-1.,0.));
#14736=DIRECTION('',(0.,-1.,0.));
#14737=DIRECTION('',(0.,0.,1.));
#14738=DIRECTION('',(0.,-1.,0.));
#14739=DIRECTION('center_axis',(0.,0.,1.));
#14740=DIRECTION('ref_axis',(1.,0.,0.));
#14741=DIRECTION('center_axis',(0.,0.,-1.));
#14742=DIRECTION('ref_axis',(1.,0.,0.));
#14743=DIRECTION('',(1.,0.,0.));
#14744=DIRECTION('',(0.,1.,0.));
#14745=DIRECTION('',(-1.,0.,0.));
#14746=DIRECTION('center_axis',(0.,0.,1.));
#14747=DIRECTION('ref_axis',(1.,0.,0.));
#14748=DIRECTION('center_axis',(0.,0.,1.));
#14749=DIRECTION('ref_axis',(1.,0.,0.));
#14750=DIRECTION('center_axis',(0.,1.,0.));
#14751=DIRECTION('ref_axis',(-1.,0.,0.));
#14752=DIRECTION('',(-1.,0.,0.));
#14753=DIRECTION('',(0.,0.,1.));
#14754=DIRECTION('center_axis',(1.,0.,0.));
#14755=DIRECTION('ref_axis',(0.,1.,0.));
#14756=DIRECTION('',(0.,1.,0.));
#14757=DIRECTION('',(0.,0.,1.));
#14758=DIRECTION('center_axis',(0.,-1.,0.));
#14759=DIRECTION('ref_axis',(1.,0.,0.));
#14760=DIRECTION('',(1.,0.,0.));
#14761=DIRECTION('center_axis',(0.,0.,1.));
#14762=DIRECTION('ref_axis',(1.,0.,0.));
#14763=DIRECTION('axis',(0.,0.,1.));
#14764=DIRECTION('refdir',(1.,0.,0.));
#14765=DIRECTION('center_axis',(0.,0.,1.));
#14766=DIRECTION('ref_axis',(1.,0.,0.));
#14767=DIRECTION('center_axis',(0.,0.,1.));
#14768=DIRECTION('ref_axis',(1.,0.,0.));
#14769=DIRECTION('',(0.,0.,1.));
#14770=DIRECTION('center_axis',(0.,0.,-1.));
#14771=DIRECTION('ref_axis',(1.,0.,0.));
#14772=DIRECTION('center_axis',(0.,0.,1.));
#14773=DIRECTION('ref_axis',(1.,0.,0.));
#14774=DIRECTION('center_axis',(0.,0.,1.));
#14775=DIRECTION('ref_axis',(1.,0.,0.));
#14776=DIRECTION('center_axis',(0.,0.,1.));
#14777=DIRECTION('ref_axis',(1.,0.,0.));
#14778=DIRECTION('center_axis',(0.,0.,1.));
#14779=DIRECTION('ref_axis',(1.,0.,0.));
#14780=DIRECTION('',(0.,0.,1.));
#14781=DIRECTION('center_axis',(0.,0.,-1.));
#14782=DIRECTION('ref_axis',(1.,0.,0.));
#14783=DIRECTION('center_axis',(0.,0.,1.));
#14784=DIRECTION('ref_axis',(1.,0.,0.));
#14785=DIRECTION('center_axis',(0.,0.,1.));
#14786=DIRECTION('ref_axis',(1.,0.,0.));
#14787=DIRECTION('center_axis',(0.,0.,1.));
#14788=DIRECTION('ref_axis',(1.,0.,0.));
#14789=DIRECTION('center_axis',(0.,0.,1.));
#14790=DIRECTION('ref_axis',(1.,0.,0.));
#14791=DIRECTION('',(0.,0.,1.));
#14792=DIRECTION('center_axis',(0.,0.,1.));
#14793=DIRECTION('ref_axis',(1.,0.,0.));
#14794=DIRECTION('center_axis',(0.,0.,1.));
#14795=DIRECTION('ref_axis',(1.,0.,0.));
#14796=DIRECTION('',(0.,0.,1.));
#14797=DIRECTION('center_axis',(0.,0.,1.));
#14798=DIRECTION('ref_axis',(1.,0.,0.));
#14799=DIRECTION('center_axis',(0.,0.,1.));
#14800=DIRECTION('ref_axis',(1.,0.,0.));
#14801=DIRECTION('',(0.,0.,-1.));
#14802=DIRECTION('center_axis',(0.,0.,1.));
#14803=DIRECTION('ref_axis',(1.,0.,0.));
#14804=DIRECTION('center_axis',(0.,0.,1.));
#14805=DIRECTION('ref_axis',(1.,0.,0.));
#14806=DIRECTION('center_axis',(0.,0.,1.));
#14807=DIRECTION('ref_axis',(1.,0.,0.));
#14808=DIRECTION('axis',(0.,0.,1.));
#14809=DIRECTION('refdir',(1.,0.,0.));
#14810=DIRECTION('center_axis',(0.,0.,1.));
#14811=DIRECTION('ref_axis',(1.,0.,0.));
#14812=DIRECTION('center_axis',(0.,0.,-1.));
#14813=DIRECTION('ref_axis',(1.,0.,0.));
#14814=DIRECTION('',(0.,0.,1.));
#14815=DIRECTION('center_axis',(0.,0.,1.));
#14816=DIRECTION('ref_axis',(1.,0.,0.));
#14817=DIRECTION('',(0.,0.,-1.));
#14818=DIRECTION('center_axis',(0.,0.,1.));
#14819=DIRECTION('ref_axis',(1.,0.,0.));
#14820=DIRECTION('',(0.,1.,0.));
#14821=DIRECTION('',(1.,0.,0.));
#14822=DIRECTION('',(0.,1.,0.));
#14823=DIRECTION('',(-1.,0.,0.));
#14824=DIRECTION('center_axis',(0.,0.,1.));
#14825=DIRECTION('ref_axis',(1.,0.,0.));
#14826=DIRECTION('center_axis',(0.,0.,1.));
#14827=DIRECTION('ref_axis',(1.,0.,0.));
#14828=DIRECTION('center_axis',(1.,0.,0.));
#14829=DIRECTION('ref_axis',(0.,0.,-1.));
#14830=DIRECTION('',(0.,1.,0.));
#14831=DIRECTION('',(0.,0.,1.));
#14832=DIRECTION('center_axis',(0.,1.,0.));
#14833=DIRECTION('ref_axis',(1.,0.,0.));
#14834=DIRECTION('center_axis',(0.,1.,0.));
#14835=DIRECTION('ref_axis',(1.,0.,0.));
#14836=DIRECTION('',(0.,1.,0.));
#14837=DIRECTION('center_axis',(0.,-1.,0.));
#14838=DIRECTION('ref_axis',(1.,0.,0.));
#14839=DIRECTION('center_axis',(0.,1.,0.));
#14840=DIRECTION('ref_axis',(1.,0.,0.));
#14841=DIRECTION('center_axis',(0.,1.,0.));
#14842=DIRECTION('ref_axis',(1.,0.,0.));
#14843=DIRECTION('',(0.,1.,0.));
#14844=DIRECTION('center_axis',(0.,-1.,0.));
#14845=DIRECTION('ref_axis',(1.,0.,0.));
#14846=DIRECTION('center_axis',(0.,1.,0.));
#14847=DIRECTION('ref_axis',(1.,0.,0.));
#14848=DIRECTION('center_axis',(0.,1.,0.));
#14849=DIRECTION('ref_axis',(1.,0.,0.));
#14850=DIRECTION('',(0.,1.,0.));
#14851=DIRECTION('center_axis',(0.,-1.,0.));
#14852=DIRECTION('ref_axis',(1.,0.,0.));
#14853=DIRECTION('center_axis',(0.,1.,0.));
#14854=DIRECTION('ref_axis',(1.,0.,0.));
#14855=DIRECTION('center_axis',(0.,1.,0.));
#14856=DIRECTION('ref_axis',(1.,0.,0.));
#14857=DIRECTION('',(0.,1.,0.));
#14858=DIRECTION('center_axis',(0.,-1.,0.));
#14859=DIRECTION('ref_axis',(1.,0.,0.));
#14860=DIRECTION('center_axis',(0.,0.,1.));
#14861=DIRECTION('ref_axis',(1.,0.,0.));
#14862=DIRECTION('',(0.,0.,1.));
#14863=DIRECTION('center_axis',(0.,0.,-1.));
#14864=DIRECTION('ref_axis',(1.,0.,0.));
#14865=DIRECTION('center_axis',(0.,0.,1.));
#14866=DIRECTION('ref_axis',(1.,0.,0.));
#14867=DIRECTION('',(0.,0.,1.));
#14868=DIRECTION('center_axis',(0.,0.,-1.));
#14869=DIRECTION('ref_axis',(1.,0.,0.));
#14870=DIRECTION('center_axis',(0.,1.,0.));
#14871=DIRECTION('ref_axis',(1.,0.,0.));
#14872=DIRECTION('center_axis',(0.,1.,0.));
#14873=DIRECTION('ref_axis',(1.,0.,0.));
#14874=DIRECTION('',(0.,1.,0.));
#14875=DIRECTION('center_axis',(0.,-1.,0.));
#14876=DIRECTION('ref_axis',(1.,0.,0.));
#14877=DIRECTION('center_axis',(0.,0.,1.));
#14878=DIRECTION('ref_axis',(1.,0.,0.));
#14879=DIRECTION('',(1.,0.,0.));
#14880=DIRECTION('',(0.,1.,0.));
#14881=DIRECTION('',(-1.,0.,0.));
#14882=DIRECTION('center_axis',(0.,0.,1.));
#14883=DIRECTION('ref_axis',(1.,0.,0.));
#14884=DIRECTION('',(0.,-1.,0.));
#14885=DIRECTION('',(1.,0.,0.));
#14886=DIRECTION('',(0.,1.,0.));
#14887=DIRECTION('',(-1.,0.,0.));
#14888=DIRECTION('center_axis',(-1.,0.,0.));
#14889=DIRECTION('ref_axis',(0.,0.,1.));
#14890=DIRECTION('',(0.,0.,-1.));
#14891=DIRECTION('',(0.,0.,1.));
#14892=DIRECTION('center_axis',(0.,-1.,0.));
#14893=DIRECTION('ref_axis',(1.,0.,0.));
#14894=DIRECTION('',(0.,0.,1.));
#14895=DIRECTION('',(1.,0.,0.));
#14896=DIRECTION('',(0.,0.,1.));
#14897=DIRECTION('center_axis',(1.,0.,0.));
#14898=DIRECTION('ref_axis',(0.,1.,0.));
#14899=DIRECTION('',(0.,0.,1.));
#14900=DIRECTION('',(0.,1.,0.));
#14901=DIRECTION('center_axis',(0.,1.,0.));
#14902=DIRECTION('ref_axis',(-1.,0.,0.));
#14903=DIRECTION('',(0.,0.,1.));
#14904=DIRECTION('',(-1.,0.,0.));
#14905=DIRECTION('center_axis',(-1.,0.,0.));
#14906=DIRECTION('ref_axis',(0.,-1.,0.));
#14907=DIRECTION('',(0.,-1.,0.));
#14908=DIRECTION('center_axis',(0.,0.,1.));
#14909=DIRECTION('ref_axis',(1.,0.,0.));
#14910=DIRECTION('axis',(0.,0.,1.));
#14911=DIRECTION('refdir',(1.,0.,0.));
#14912=DIRECTION('center_axis',(0.,1.,0.));
#14913=DIRECTION('ref_axis',(1.,0.,0.));
#14914=DIRECTION('center_axis',(0.,1.,0.));
#14915=DIRECTION('ref_axis',(1.,0.,0.));
#14916=DIRECTION('',(0.,1.,0.));
#14917=DIRECTION('center_axis',(0.,-1.,0.));
#14918=DIRECTION('ref_axis',(1.,0.,0.));
#14919=DIRECTION('center_axis',(0.,1.,0.));
#14920=DIRECTION('ref_axis',(1.,0.,0.));
#14921=DIRECTION('center_axis',(0.,1.,0.));
#14922=DIRECTION('ref_axis',(1.,0.,0.));
#14923=DIRECTION('',(0.,1.,0.));
#14924=DIRECTION('center_axis',(0.,-1.,0.));
#14925=DIRECTION('ref_axis',(1.,0.,0.));
#14926=DIRECTION('center_axis',(0.,1.,0.));
#14927=DIRECTION('ref_axis',(1.,0.,0.));
#14928=DIRECTION('center_axis',(0.,1.,0.));
#14929=DIRECTION('ref_axis',(1.,0.,0.));
#14930=DIRECTION('',(0.,1.,0.));
#14931=DIRECTION('center_axis',(0.,-1.,0.));
#14932=DIRECTION('ref_axis',(1.,0.,0.));
#14933=DIRECTION('center_axis',(0.,1.,0.));
#14934=DIRECTION('ref_axis',(1.,0.,0.));
#14935=DIRECTION('center_axis',(0.,1.,0.));
#14936=DIRECTION('ref_axis',(1.,0.,0.));
#14937=DIRECTION('',(0.,1.,0.));
#14938=DIRECTION('center_axis',(0.,-1.,0.));
#14939=DIRECTION('ref_axis',(1.,0.,0.));
#14940=DIRECTION('center_axis',(0.,1.,0.));
#14941=DIRECTION('ref_axis',(1.,0.,0.));
#14942=DIRECTION('center_axis',(0.,1.,0.));
#14943=DIRECTION('ref_axis',(1.,0.,0.));
#14944=DIRECTION('',(0.,1.,0.));
#14945=DIRECTION('center_axis',(0.,-1.,0.));
#14946=DIRECTION('ref_axis',(1.,0.,0.));
#14947=DIRECTION('center_axis',(0.,1.,0.));
#14948=DIRECTION('ref_axis',(1.,0.,0.));
#14949=DIRECTION('center_axis',(0.,1.,0.));
#14950=DIRECTION('ref_axis',(1.,0.,0.));
#14951=DIRECTION('',(0.,-1.,0.));
#14952=DIRECTION('center_axis',(0.,-1.,0.));
#14953=DIRECTION('ref_axis',(1.,0.,0.));
#14954=DIRECTION('center_axis',(0.,1.,0.));
#14955=DIRECTION('ref_axis',(1.,0.,0.));
#14956=DIRECTION('center_axis',(0.,1.,0.));
#14957=DIRECTION('ref_axis',(1.,0.,0.));
#14958=DIRECTION('center_axis',(0.,1.,0.));
#14959=DIRECTION('ref_axis',(1.,0.,0.));
#14960=DIRECTION('',(0.,-1.,0.));
#14961=DIRECTION('center_axis',(0.,1.,0.));
#14962=DIRECTION('ref_axis',(1.,0.,0.));
#14963=DIRECTION('center_axis',(0.,1.,0.));
#14964=DIRECTION('ref_axis',(1.,0.,0.));
#14965=DIRECTION('center_axis',(0.,1.,0.));
#14966=DIRECTION('ref_axis',(1.,0.,0.));
#14967=DIRECTION('axis',(0.,0.,1.));
#14968=DIRECTION('refdir',(1.,0.,0.));
#14969=DIRECTION('center_axis',(0.,1.,0.));
#14970=DIRECTION('ref_axis',(1.,0.,0.));
#14971=DIRECTION('center_axis',(0.,1.,0.));
#14972=DIRECTION('ref_axis',(1.,0.,0.));
#14973=DIRECTION('',(0.,1.,0.));
#14974=DIRECTION('center_axis',(0.,-1.,0.));
#14975=DIRECTION('ref_axis',(1.,0.,0.));
#14976=DIRECTION('center_axis',(0.,1.,0.));
#14977=DIRECTION('ref_axis',(1.,0.,0.));
#14978=DIRECTION('center_axis',(0.,1.,0.));
#14979=DIRECTION('ref_axis',(1.,0.,0.));
#14980=DIRECTION('',(0.,1.,0.));
#14981=DIRECTION('center_axis',(0.,-1.,0.));
#14982=DIRECTION('ref_axis',(1.,0.,0.));
#14983=DIRECTION('center_axis',(0.,1.,0.));
#14984=DIRECTION('ref_axis',(1.,0.,0.));
#14985=DIRECTION('center_axis',(0.,1.,0.));
#14986=DIRECTION('ref_axis',(1.,0.,0.));
#14987=DIRECTION('',(0.,1.,0.));
#14988=DIRECTION('center_axis',(0.,-1.,0.));
#14989=DIRECTION('ref_axis',(1.,0.,0.));
#14990=DIRECTION('center_axis',(0.,1.,0.));
#14991=DIRECTION('ref_axis',(1.,0.,0.));
#14992=DIRECTION('center_axis',(0.,1.,0.));
#14993=DIRECTION('ref_axis',(1.,0.,0.));
#14994=DIRECTION('',(0.,1.,0.));
#14995=DIRECTION('center_axis',(0.,-1.,0.));
#14996=DIRECTION('ref_axis',(1.,0.,0.));
#14997=DIRECTION('center_axis',(0.,1.,0.));
#14998=DIRECTION('ref_axis',(1.,0.,0.));
#14999=DIRECTION('center_axis',(0.,1.,0.));
#15000=DIRECTION('ref_axis',(1.,0.,0.));
#15001=DIRECTION('',(0.,1.,0.));
#15002=DIRECTION('center_axis',(0.,-1.,0.));
#15003=DIRECTION('ref_axis',(1.,0.,0.));
#15004=DIRECTION('center_axis',(0.,1.,0.));
#15005=DIRECTION('ref_axis',(1.,0.,0.));
#15006=DIRECTION('center_axis',(0.,1.,0.));
#15007=DIRECTION('ref_axis',(1.,0.,0.));
#15008=DIRECTION('',(0.,-1.,0.));
#15009=DIRECTION('center_axis',(0.,1.,0.));
#15010=DIRECTION('ref_axis',(1.,0.,0.));
#15011=DIRECTION('center_axis',(0.,1.,0.));
#15012=DIRECTION('ref_axis',(1.,0.,0.));
#15013=DIRECTION('center_axis',(0.,1.,0.));
#15014=DIRECTION('ref_axis',(1.,0.,0.));
#15015=DIRECTION('center_axis',(0.,1.,0.));
#15016=DIRECTION('ref_axis',(1.,0.,0.));
#15017=DIRECTION('',(0.,-1.,0.));
#15018=DIRECTION('center_axis',(0.,1.,0.));
#15019=DIRECTION('ref_axis',(1.,0.,0.));
#15020=DIRECTION('center_axis',(0.,1.,0.));
#15021=DIRECTION('ref_axis',(1.,0.,0.));
#15022=DIRECTION('center_axis',(0.,1.,0.));
#15023=DIRECTION('ref_axis',(1.,0.,0.));
#15024=DIRECTION('axis',(0.,0.,1.));
#15025=DIRECTION('refdir',(1.,0.,0.));
#15026=DIRECTION('center_axis',(0.,0.,1.));
#15027=DIRECTION('ref_axis',(1.,0.,0.));
#15028=DIRECTION('center_axis',(0.,0.,-1.));
#15029=DIRECTION('ref_axis',(1.,0.,0.));
#15030=DIRECTION('',(0.,0.,1.));
#15031=DIRECTION('center_axis',(0.,0.,1.));
#15032=DIRECTION('ref_axis',(1.,0.,0.));
#15033=DIRECTION('',(0.,0.,-1.));
#15034=DIRECTION('center_axis',(0.,0.,1.));
#15035=DIRECTION('ref_axis',(1.,0.,0.));
#15036=DIRECTION('',(1.,0.,0.));
#15037=DIRECTION('',(0.,1.,0.));
#15038=DIRECTION('',(-1.,0.,0.));
#15039=DIRECTION('',(0.,1.,0.));
#15040=DIRECTION('center_axis',(0.,0.,1.));
#15041=DIRECTION('ref_axis',(1.,0.,0.));
#15042=DIRECTION('center_axis',(0.,0.,1.));
#15043=DIRECTION('ref_axis',(1.,0.,0.));
#15044=DIRECTION('center_axis',(0.,-1.,0.));
#15045=DIRECTION('ref_axis',(1.,0.,0.));
#15046=DIRECTION('',(-1.,0.,0.));
#15047=DIRECTION('',(0.,0.,1.));
#15048=DIRECTION('',(1.,0.,0.));
#15049=DIRECTION('',(0.,0.,1.));
#15050=DIRECTION('',(-1.,0.,0.));
#15051=DIRECTION('',(0.,0.,-1.));
#15052=DIRECTION('center_axis',(0.,1.,0.));
#15053=DIRECTION('ref_axis',(1.,0.,0.));
#15054=DIRECTION('center_axis',(0.,1.,0.));
#15055=DIRECTION('ref_axis',(1.,0.,0.));
#15056=DIRECTION('center_axis',(0.,1.,0.));
#15057=DIRECTION('ref_axis',(1.,0.,0.));
#15058=DIRECTION('center_axis',(0.,1.,0.));
#15059=DIRECTION('ref_axis',(1.,0.,0.));
#15060=DIRECTION('center_axis',(0.,1.,0.));
#15061=DIRECTION('ref_axis',(1.,0.,0.));
#15062=DIRECTION('center_axis',(0.,1.,0.));
#15063=DIRECTION('ref_axis',(1.,0.,0.));
#15064=DIRECTION('',(0.,1.,0.));
#15065=DIRECTION('center_axis',(0.,-1.,0.));
#15066=DIRECTION('ref_axis',(1.,0.,0.));
#15067=DIRECTION('center_axis',(0.,1.,0.));
#15068=DIRECTION('ref_axis',(1.,0.,0.));
#15069=DIRECTION('',(0.,1.,0.));
#15070=DIRECTION('center_axis',(0.,-1.,0.));
#15071=DIRECTION('ref_axis',(1.,0.,0.));
#15072=DIRECTION('center_axis',(0.,1.,0.));
#15073=DIRECTION('ref_axis',(1.,0.,0.));
#15074=DIRECTION('',(0.,1.,0.));
#15075=DIRECTION('center_axis',(0.,-1.,0.));
#15076=DIRECTION('ref_axis',(1.,0.,0.));
#15077=DIRECTION('center_axis',(0.,1.,0.));
#15078=DIRECTION('ref_axis',(1.,0.,0.));
#15079=DIRECTION('',(0.,1.,0.));
#15080=DIRECTION('center_axis',(0.,-1.,0.));
#15081=DIRECTION('ref_axis',(1.,0.,0.));
#15082=DIRECTION('center_axis',(0.,0.,1.));
#15083=DIRECTION('ref_axis',(1.,0.,0.));
#15084=DIRECTION('',(0.,0.,1.));
#15085=DIRECTION('center_axis',(0.,0.,-1.));
#15086=DIRECTION('ref_axis',(1.,0.,0.));
#15087=DIRECTION('center_axis',(0.,0.,1.));
#15088=DIRECTION('ref_axis',(1.,0.,0.));
#15089=DIRECTION('',(0.,0.,1.));
#15090=DIRECTION('center_axis',(0.,0.,-1.));
#15091=DIRECTION('ref_axis',(1.,0.,0.));
#15092=DIRECTION('center_axis',(0.,1.,0.));
#15093=DIRECTION('ref_axis',(1.,0.,0.));
#15094=DIRECTION('',(0.,1.,0.));
#15095=DIRECTION('center_axis',(0.,-1.,0.));
#15096=DIRECTION('ref_axis',(1.,0.,0.));
#15097=DIRECTION('center_axis',(0.,0.,1.));
#15098=DIRECTION('ref_axis',(1.,0.,0.));
#15099=DIRECTION('',(0.,1.,0.));
#15100=DIRECTION('',(1.,0.,0.));
#15101=DIRECTION('',(0.,1.,0.));
#15102=DIRECTION('center_axis',(0.,0.,1.));
#15103=DIRECTION('ref_axis',(1.,0.,0.));
#15104=DIRECTION('',(0.,-1.,0.));
#15105=DIRECTION('',(1.,0.,0.));
#15106=DIRECTION('',(0.,1.,0.));
#15107=DIRECTION('center_axis',(-1.,0.,0.));
#15108=DIRECTION('ref_axis',(0.,0.,1.));
#15109=DIRECTION('',(0.,0.,1.));
#15110=DIRECTION('center_axis',(1.,0.,0.));
#15111=DIRECTION('ref_axis',(0.,0.,-1.));
#15112=DIRECTION('',(0.,0.,-1.));
#15113=DIRECTION('center_axis',(1.,0.,0.));
#15114=DIRECTION('ref_axis',(0.,1.,0.));
#15115=DIRECTION('',(0.,0.,1.));
#15116=DIRECTION('',(0.,1.,0.));
#15117=DIRECTION('center_axis',(0.,1.,0.));
#15118=DIRECTION('ref_axis',(-1.,0.,0.));
#15119=DIRECTION('',(0.,0.,1.));
#15120=DIRECTION('',(-1.,0.,0.));
#15121=DIRECTION('center_axis',(-1.,0.,0.));
#15122=DIRECTION('ref_axis',(0.,-1.,0.));
#15123=DIRECTION('',(0.,-1.,0.));
#15124=DIRECTION('center_axis',(0.,0.,1.));
#15125=DIRECTION('ref_axis',(1.,0.,0.));
#15126=DIRECTION('axis',(0.,0.,1.));
#15127=DIRECTION('refdir',(1.,0.,0.));
#15128=DIRECTION('center_axis',(0.,1.,0.));
#15129=DIRECTION('ref_axis',(1.,0.,0.));
#15130=DIRECTION('center_axis',(0.,1.,0.));
#15131=DIRECTION('ref_axis',(1.,0.,0.));
#15132=DIRECTION('',(0.,1.,0.));
#15133=DIRECTION('center_axis',(0.,-1.,0.));
#15134=DIRECTION('ref_axis',(1.,0.,0.));
#15135=DIRECTION('center_axis',(0.,1.,0.));
#15136=DIRECTION('ref_axis',(1.,0.,0.));
#15137=DIRECTION('center_axis',(0.,1.,0.));
#15138=DIRECTION('ref_axis',(1.,0.,0.));
#15139=DIRECTION('',(0.,1.,0.));
#15140=DIRECTION('center_axis',(0.,-1.,0.));
#15141=DIRECTION('ref_axis',(1.,0.,0.));
#15142=DIRECTION('center_axis',(0.,1.,0.));
#15143=DIRECTION('ref_axis',(1.,0.,0.));
#15144=DIRECTION('center_axis',(0.,1.,0.));
#15145=DIRECTION('ref_axis',(1.,0.,0.));
#15146=DIRECTION('',(0.,1.,0.));
#15147=DIRECTION('center_axis',(0.,-1.,0.));
#15148=DIRECTION('ref_axis',(1.,0.,0.));
#15149=DIRECTION('center_axis',(0.,1.,0.));
#15150=DIRECTION('ref_axis',(1.,0.,0.));
#15151=DIRECTION('center_axis',(0.,1.,0.));
#15152=DIRECTION('ref_axis',(1.,0.,0.));
#15153=DIRECTION('',(0.,1.,0.));
#15154=DIRECTION('center_axis',(0.,-1.,0.));
#15155=DIRECTION('ref_axis',(1.,0.,0.));
#15156=DIRECTION('center_axis',(0.,1.,0.));
#15157=DIRECTION('ref_axis',(1.,0.,0.));
#15158=DIRECTION('center_axis',(0.,1.,0.));
#15159=DIRECTION('ref_axis',(1.,0.,0.));
#15160=DIRECTION('',(0.,1.,0.));
#15161=DIRECTION('center_axis',(0.,-1.,0.));
#15162=DIRECTION('ref_axis',(1.,0.,0.));
#15163=DIRECTION('center_axis',(0.,1.,0.));
#15164=DIRECTION('ref_axis',(1.,0.,0.));
#15165=DIRECTION('center_axis',(0.,1.,0.));
#15166=DIRECTION('ref_axis',(1.,0.,0.));
#15167=DIRECTION('',(0.,-1.,0.));
#15168=DIRECTION('center_axis',(0.,-1.,0.));
#15169=DIRECTION('ref_axis',(1.,0.,0.));
#15170=DIRECTION('center_axis',(0.,1.,0.));
#15171=DIRECTION('ref_axis',(1.,0.,0.));
#15172=DIRECTION('center_axis',(0.,1.,0.));
#15173=DIRECTION('ref_axis',(1.,0.,0.));
#15174=DIRECTION('center_axis',(0.,1.,0.));
#15175=DIRECTION('ref_axis',(1.,0.,0.));
#15176=DIRECTION('',(0.,-1.,0.));
#15177=DIRECTION('center_axis',(0.,1.,0.));
#15178=DIRECTION('ref_axis',(1.,0.,0.));
#15179=DIRECTION('center_axis',(0.,1.,0.));
#15180=DIRECTION('ref_axis',(1.,0.,0.));
#15181=DIRECTION('center_axis',(0.,1.,0.));
#15182=DIRECTION('ref_axis',(1.,0.,0.));
#15183=DIRECTION('axis',(0.,0.,1.));
#15184=DIRECTION('refdir',(1.,0.,0.));
#15185=DIRECTION('center_axis',(0.,1.,0.));
#15186=DIRECTION('ref_axis',(1.,0.,0.));
#15187=DIRECTION('center_axis',(0.,1.,0.));
#15188=DIRECTION('ref_axis',(1.,0.,0.));
#15189=DIRECTION('',(0.,1.,0.));
#15190=DIRECTION('center_axis',(0.,-1.,0.));
#15191=DIRECTION('ref_axis',(1.,0.,0.));
#15192=DIRECTION('center_axis',(0.,1.,0.));
#15193=DIRECTION('ref_axis',(1.,0.,0.));
#15194=DIRECTION('center_axis',(0.,1.,0.));
#15195=DIRECTION('ref_axis',(1.,0.,0.));
#15196=DIRECTION('',(0.,1.,0.));
#15197=DIRECTION('center_axis',(0.,-1.,0.));
#15198=DIRECTION('ref_axis',(1.,0.,0.));
#15199=DIRECTION('center_axis',(0.,1.,0.));
#15200=DIRECTION('ref_axis',(1.,0.,0.));
#15201=DIRECTION('center_axis',(0.,1.,0.));
#15202=DIRECTION('ref_axis',(1.,0.,0.));
#15203=DIRECTION('',(0.,1.,0.));
#15204=DIRECTION('center_axis',(0.,-1.,0.));
#15205=DIRECTION('ref_axis',(1.,0.,0.));
#15206=DIRECTION('center_axis',(0.,1.,0.));
#15207=DIRECTION('ref_axis',(1.,0.,0.));
#15208=DIRECTION('center_axis',(0.,1.,0.));
#15209=DIRECTION('ref_axis',(1.,0.,0.));
#15210=DIRECTION('',(0.,1.,0.));
#15211=DIRECTION('center_axis',(0.,-1.,0.));
#15212=DIRECTION('ref_axis',(1.,0.,0.));
#15213=DIRECTION('center_axis',(0.,1.,0.));
#15214=DIRECTION('ref_axis',(1.,0.,0.));
#15215=DIRECTION('center_axis',(0.,1.,0.));
#15216=DIRECTION('ref_axis',(1.,0.,0.));
#15217=DIRECTION('',(0.,1.,0.));
#15218=DIRECTION('center_axis',(0.,-1.,0.));
#15219=DIRECTION('ref_axis',(1.,0.,0.));
#15220=DIRECTION('center_axis',(0.,1.,0.));
#15221=DIRECTION('ref_axis',(1.,0.,0.));
#15222=DIRECTION('center_axis',(0.,1.,0.));
#15223=DIRECTION('ref_axis',(1.,0.,0.));
#15224=DIRECTION('',(0.,-1.,0.));
#15225=DIRECTION('center_axis',(0.,1.,0.));
#15226=DIRECTION('ref_axis',(1.,0.,0.));
#15227=DIRECTION('center_axis',(0.,1.,0.));
#15228=DIRECTION('ref_axis',(1.,0.,0.));
#15229=DIRECTION('center_axis',(0.,1.,0.));
#15230=DIRECTION('ref_axis',(1.,0.,0.));
#15231=DIRECTION('center_axis',(0.,1.,0.));
#15232=DIRECTION('ref_axis',(1.,0.,0.));
#15233=DIRECTION('',(0.,-1.,0.));
#15234=DIRECTION('center_axis',(0.,1.,0.));
#15235=DIRECTION('ref_axis',(1.,0.,0.));
#15236=DIRECTION('center_axis',(0.,1.,0.));
#15237=DIRECTION('ref_axis',(1.,0.,0.));
#15238=DIRECTION('center_axis',(0.,1.,0.));
#15239=DIRECTION('ref_axis',(1.,0.,0.));
#15240=DIRECTION('axis',(0.,0.,1.));
#15241=DIRECTION('refdir',(1.,0.,0.));
#15242=DIRECTION('center_axis',(0.,1.,0.));
#15243=DIRECTION('ref_axis',(0.,0.,1.));
#15244=DIRECTION('center_axis',(0.,-1.,0.));
#15245=DIRECTION('ref_axis',(1.,0.,0.));
#15246=DIRECTION('center_axis',(0.,-1.,0.));
#15247=DIRECTION('ref_axis',(1.,0.,0.));
#15248=DIRECTION('center_axis',(0.,-1.,0.));
#15249=DIRECTION('ref_axis',(1.,0.,0.));
#15250=DIRECTION('',(0.707106781186548,0.707106781186547,8.65956056235493E-17));
#15251=DIRECTION('center_axis',(0.,-1.,0.));
#15252=DIRECTION('ref_axis',(1.,0.,0.));
#15253=DIRECTION('center_axis',(0.,-1.,0.));
#15254=DIRECTION('ref_axis',(1.,0.,0.));
#15255=DIRECTION('',(0.,1.,0.));
#15256=DIRECTION('center_axis',(0.,1.,0.));
#15257=DIRECTION('ref_axis',(1.,0.,0.));
#15258=DIRECTION('center_axis',(0.,-1.,0.));
#15259=DIRECTION('ref_axis',(1.,0.,0.));
#15260=DIRECTION('',(-0.707106781186547,0.707106781186548,-8.65956056235493E-17));
#15261=DIRECTION('center_axis',(0.,-1.,0.));
#15262=DIRECTION('ref_axis',(0.,0.,-1.));
#15263=DIRECTION('center_axis',(0.,-1.,0.));
#15264=DIRECTION('ref_axis',(1.,0.,0.));
#15265=DIRECTION('center_axis',(0.,1.,0.));
#15266=DIRECTION('ref_axis',(1.,0.,0.));
#15267=DIRECTION('center_axis',(0.,1.,0.));
#15268=DIRECTION('ref_axis',(1.,0.,0.));
#15269=DIRECTION('',(-0.447213595499958,0.894427190999916,-5.47678698264203E-17));
#15270=DIRECTION('center_axis',(0.,-1.,0.));
#15271=DIRECTION('ref_axis',(1.,0.,0.));
#15272=DIRECTION('center_axis',(0.,1.,0.));
#15273=DIRECTION('ref_axis',(1.,0.,0.));
#15274=DIRECTION('',(0.,1.,0.));
#15275=DIRECTION('center_axis',(0.,1.,0.));
#15276=DIRECTION('ref_axis',(1.,0.,0.));
#15277=DIRECTION('center_axis',(0.,-1.,0.));
#15278=DIRECTION('ref_axis',(1.,0.,0.));
#15279=DIRECTION('',(-0.707106781186547,0.707106781186548,-8.65956056235493E-17));
#15280=DIRECTION('center_axis',(0.,-1.,0.));
#15281=DIRECTION('ref_axis',(0.,0.,-1.));
#15282=DIRECTION('center_axis',(0.866025403784439,0.,-0.5));
#15283=DIRECTION('ref_axis',(0.5,0.,0.866025403784439));
#15284=DIRECTION('',(-0.5,0.,-0.866025403784439));
#15285=DIRECTION('',(0.,-1.,0.));
#15286=DIRECTION('',(0.5,0.,0.866025403784439));
#15287=DIRECTION('',(0.,-1.,0.));
#15288=DIRECTION('center_axis',(1.20185167898973E-16,0.,-1.));
#15289=DIRECTION('ref_axis',(1.,0.,1.20185167898973E-16));
#15290=DIRECTION('',(-1.,0.,-1.20185167898973E-16));
#15291=DIRECTION('',(0.,-1.,0.));
#15292=DIRECTION('',(1.,0.,1.20185167898973E-16));
#15293=DIRECTION('center_axis',(-0.866025403784439,0.,-0.5));
#15294=DIRECTION('ref_axis',(0.5,0.,-0.866025403784439));
#15295=DIRECTION('',(-0.5,0.,0.866025403784439));
#15296=DIRECTION('',(0.,-1.,0.));
#15297=DIRECTION('',(0.5,0.,-0.866025403784439));
#15298=DIRECTION('center_axis',(-0.866025403784439,0.,0.5));
#15299=DIRECTION('ref_axis',(-0.5,0.,-0.866025403784439));
#15300=DIRECTION('',(0.5,0.,0.866025403784439));
#15301=DIRECTION('',(0.,-1.,0.));
#15302=DIRECTION('',(-0.5,0.,-0.866025403784439));
#15303=DIRECTION('center_axis',(-2.40370335797945E-16,0.,1.));
#15304=DIRECTION('ref_axis',(-1.,0.,-2.40370335797945E-16));
#15305=DIRECTION('',(1.,0.,2.40370335797945E-16));
#15306=DIRECTION('',(0.,-1.,0.));
#15307=DIRECTION('',(-1.,0.,-2.40370335797945E-16));
#15308=DIRECTION('center_axis',(0.866025403784439,0.,0.5));
#15309=DIRECTION('ref_axis',(-0.5,0.,0.866025403784439));
#15310=DIRECTION('',(0.5,0.,-0.866025403784439));
#15311=DIRECTION('',(-0.5,0.,0.866025403784439));
#15312=DIRECTION('center_axis',(0.,1.,0.));
#15313=DIRECTION('ref_axis',(1.,0.,0.));
#15314=DIRECTION('center_axis',(0.,-1.,0.));
#15315=DIRECTION('ref_axis',(0.,0.,-1.));
#15316=DIRECTION('axis',(0.,0.,1.));
#15317=DIRECTION('refdir',(1.,0.,0.));
#15318=DIRECTION('axis',(0.,0.,1.));
#15319=DIRECTION('refdir',(1.,0.,0.));
#15320=DIRECTION('center_axis',(0.,-1.,0.));
#15321=DIRECTION('ref_axis',(0.,0.,-1.));
#15322=DIRECTION('center_axis',(0.,-1.,0.));
#15323=DIRECTION('ref_axis',(1.,0.,0.));
#15324=DIRECTION('center_axis',(0.,-1.,0.));
#15325=DIRECTION('ref_axis',(1.,0.,0.));
#15326=DIRECTION('center_axis',(1.,0.,1.22464679914735E-16));
#15327=DIRECTION('ref_axis',(-1.22464679914735E-16,0.,1.));
#15328=DIRECTION('center_axis',(0.,1.,0.));
#15329=DIRECTION('ref_axis',(1.,0.,0.));
#15330=DIRECTION('center_axis',(0.,1.,0.));
#15331=DIRECTION('ref_axis',(1.,0.,0.));
#15332=DIRECTION('center_axis',(0.,-1.,0.));
#15333=DIRECTION('ref_axis',(1.,0.,0.));
#15334=DIRECTION('',(0.,1.,0.));
#15335=DIRECTION('center_axis',(0.,-1.,0.));
#15336=DIRECTION('ref_axis',(1.,0.,0.));
#15337=DIRECTION('center_axis',(0.,-1.,0.));
#15338=DIRECTION('ref_axis',(1.,0.,0.));
#15339=DIRECTION('center_axis',(0.,-1.,0.));
#15340=DIRECTION('ref_axis',(1.,0.,0.));
#15341=DIRECTION('',(0.,1.,0.));
#15342=DIRECTION('center_axis',(0.,-1.,0.));
#15343=DIRECTION('ref_axis',(1.,0.,0.));
#15344=DIRECTION('center_axis',(0.,1.,0.));
#15345=DIRECTION('ref_axis',(1.,0.,0.));
#15346=DIRECTION('',(-0.707106781186548,0.707106781186547,-8.65956056235493E-17));
#15347=DIRECTION('center_axis',(0.,-1.,0.));
#15348=DIRECTION('ref_axis',(1.,0.,0.));
#15349=DIRECTION('center_axis',(0.,1.,0.));
#15350=DIRECTION('ref_axis',(0.,0.,1.));
#15351=DIRECTION('center_axis',(0.,-1.,0.));
#15352=DIRECTION('ref_axis',(1.,0.,0.));
#15353=DIRECTION('center_axis',(0.,-1.,0.));
#15354=DIRECTION('ref_axis',(1.,0.,0.));
#15355=DIRECTION('',(0.,1.,0.));
#15356=DIRECTION('center_axis',(0.,-1.,0.));
#15357=DIRECTION('ref_axis',(0.,0.,-1.));
#15358=DIRECTION('center_axis',(0.,-1.,0.));
#15359=DIRECTION('ref_axis',(1.,0.,0.));
#15360=DIRECTION('center_axis',(0.,-1.,0.));
#15361=DIRECTION('ref_axis',(1.,0.,0.));
#15362=DIRECTION('',(0.707106781186548,0.707106781186547,8.65956056235493E-17));
#15363=DIRECTION('axis',(0.,0.,1.));
#15364=DIRECTION('refdir',(1.,0.,0.));
#15365=DIRECTION('center_axis',(0.,-1.,0.));
#15366=DIRECTION('ref_axis',(0.,0.,-1.));
#15367=DIRECTION('center_axis',(0.,-1.,0.));
#15368=DIRECTION('ref_axis',(1.,0.,0.));
#15369=DIRECTION('center_axis',(0.,-1.,0.));
#15370=DIRECTION('ref_axis',(1.,0.,0.));
#15371=DIRECTION('center_axis',(1.,0.,1.22464679914735E-16));
#15372=DIRECTION('ref_axis',(-1.22464679914735E-16,0.,1.));
#15373=DIRECTION('center_axis',(0.,1.,0.));
#15374=DIRECTION('ref_axis',(1.,0.,0.));
#15375=DIRECTION('center_axis',(0.,1.,0.));
#15376=DIRECTION('ref_axis',(1.,0.,0.));
#15377=DIRECTION('center_axis',(0.,-1.,0.));
#15378=DIRECTION('ref_axis',(1.,0.,0.));
#15379=DIRECTION('center_axis',(0.,-1.,0.));
#15380=DIRECTION('ref_axis',(1.,0.,0.));
#15381=DIRECTION('',(0.,1.,0.));
#15382=DIRECTION('center_axis',(0.,1.,0.));
#15383=DIRECTION('ref_axis',(0.,0.,1.));
#15384=DIRECTION('center_axis',(0.,-1.,0.));
#15385=DIRECTION('ref_axis',(1.,0.,0.));
#15386=DIRECTION('center_axis',(0.,-1.,0.));
#15387=DIRECTION('ref_axis',(1.,0.,0.));
#15388=DIRECTION('center_axis',(0.,-1.,0.));
#15389=DIRECTION('ref_axis',(1.,0.,0.));
#15390=DIRECTION('center_axis',(0.,-1.,0.));
#15391=DIRECTION('ref_axis',(1.,0.,0.));
#15392=DIRECTION('',(0.707106781186548,0.707106781186547,8.65956056235494E-17));
#15393=DIRECTION('center_axis',(0.,-1.,0.));
#15394=DIRECTION('ref_axis',(1.,0.,0.));
#15395=DIRECTION('center_axis',(0.,-1.,0.));
#15396=DIRECTION('ref_axis',(1.,0.,0.));
#15397=DIRECTION('',(0.,1.,0.));
#15398=DIRECTION('center_axis',(0.,1.,0.));
#15399=DIRECTION('ref_axis',(1.,0.,0.));
#15400=DIRECTION('center_axis',(0.,-1.,0.));
#15401=DIRECTION('ref_axis',(1.,0.,0.));
#15402=DIRECTION('',(-0.707106781186548,0.707106781186547,-8.65956056235494E-17));
#15403=DIRECTION('center_axis',(0.,-1.,0.));
#15404=DIRECTION('ref_axis',(0.,0.,-1.));
#15405=DIRECTION('center_axis',(0.,-1.,0.));
#15406=DIRECTION('ref_axis',(1.,0.,0.));
#15407=DIRECTION('',(0.,1.,0.));
#15408=DIRECTION('axis',(0.,0.,1.));
#15409=DIRECTION('refdir',(1.,0.,0.));
#15410=DIRECTION('center_axis',(0.,0.,1.));
#15411=DIRECTION('ref_axis',(1.,0.,0.));
#15412=DIRECTION('center_axis',(1.22464679914735E-16,-1.,0.));
#15413=DIRECTION('ref_axis',(-1.,-1.22464679914735E-16,0.));
#15414=DIRECTION('center_axis',(0.78183148246803,0.,0.623489801858733));
#15415=DIRECTION('ref_axis',(0.623489801858734,0.,-0.78183148246803));
#15416=DIRECTION('center_axis',(7.63554790147315E-17,-1.,-9.57467422477103E-17));
#15417=DIRECTION('ref_axis',(-0.623489801858734,-1.22464679914735E-16,0.78183148246803));
#15418=DIRECTION('center_axis',(0.974927912181824,0.,-0.222520933956314));
#15419=DIRECTION('ref_axis',(-0.222520933956314,0.,-0.974927912181824));
#15420=DIRECTION('center_axis',(-2.7250954951288E-17,-1.,-1.19394234705288E-16));
#15421=DIRECTION('ref_axis',(0.222520933956314,-1.22464679914735E-16,0.974927912181824));
#15422=DIRECTION('center_axis',(0.433883739117558,0.,-0.900968867902419));
#15423=DIRECTION('ref_axis',(-0.900968867902419,0.,-0.433883739117558));
#15424=DIRECTION('center_axis',(-1.10336864020811E-16,-1.,-5.31354332312403E-17));
#15425=DIRECTION('ref_axis',(0.900968867902419,-1.22464679914735E-16,0.433883739117558));
#15426=DIRECTION('center_axis',(-0.433883739117558,0.,-0.900968867902419));
#15427=DIRECTION('ref_axis',(-0.900968867902419,0.,0.433883739117558));
#15428=DIRECTION('center_axis',(-1.10336864020811E-16,-1.,5.31354332312403E-17));
#15429=DIRECTION('ref_axis',(0.900968867902419,-1.22464679914735E-16,-0.433883739117558));
#15430=DIRECTION('center_axis',(-0.974927912181824,0.,-0.222520933956314));
#15431=DIRECTION('ref_axis',(-0.222520933956315,0.,0.974927912181824));
#15432=DIRECTION('center_axis',(-2.7250954951288E-17,-1.,1.19394234705288E-16));
#15433=DIRECTION('ref_axis',(0.222520933956315,-1.22464679914735E-16,-0.974927912181824));
#15434=DIRECTION('center_axis',(-0.78183148246803,0.,0.623489801858734));
#15435=DIRECTION('ref_axis',(0.623489801858733,0.,0.78183148246803));
#15436=DIRECTION('center_axis',(7.63554790147315E-17,-1.,9.57467422477103E-17));
#15437=DIRECTION('ref_axis',(-0.623489801858733,-1.22464679914735E-16,-0.78183148246803));
#15438=DIRECTION('axis',(0.,0.,1.));
#15439=DIRECTION('refdir',(1.,0.,0.));
#15440=DIRECTION('center_axis',(0.,0.,1.));
#15441=DIRECTION('ref_axis',(1.,0.,0.));
#15442=DIRECTION('center_axis',(0.,-1.,0.));
#15443=DIRECTION('ref_axis',(0.,0.,-1.));
#15444=DIRECTION('center_axis',(0.,-1.,0.));
#15445=DIRECTION('ref_axis',(0.,0.,-1.));
#15446=DIRECTION('center_axis',(0.,1.,0.));
#15447=DIRECTION('ref_axis',(1.,0.,0.));
#15448=DIRECTION('center_axis',(0.,1.,0.));
#15449=DIRECTION('ref_axis',(1.,0.,0.));
#15450=DIRECTION('center_axis',(0.,1.,0.));
#15451=DIRECTION('ref_axis',(1.,0.,0.));
#15452=DIRECTION('center_axis',(0.,1.,0.));
#15453=DIRECTION('ref_axis',(1.,0.,0.));
#15454=DIRECTION('',(0.,-1.,0.));
#15455=DIRECTION('center_axis',(0.,-1.,0.));
#15456=DIRECTION('ref_axis',(1.,0.,0.));
#15457=DIRECTION('center_axis',(0.,1.,0.));
#15458=DIRECTION('ref_axis',(1.,0.,0.));
#15459=DIRECTION('center_axis',(0.,1.,0.));
#15460=DIRECTION('ref_axis',(1.,0.,0.));
#15461=DIRECTION('center_axis',(0.,1.,0.));
#15462=DIRECTION('ref_axis',(1.,0.,0.));
#15463=DIRECTION('center_axis',(0.,1.,0.));
#15464=DIRECTION('ref_axis',(1.,0.,0.));
#15465=DIRECTION('center_axis',(0.,1.,0.));
#15466=DIRECTION('ref_axis',(1.,0.,0.));
#15467=DIRECTION('center_axis',(0.,1.,0.));
#15468=DIRECTION('ref_axis',(1.,0.,0.));
#15469=DIRECTION('center_axis',(0.,-1.,0.));
#15470=DIRECTION('ref_axis',(1.,0.,0.));
#15471=DIRECTION('center_axis',(0.,-1.,0.));
#15472=DIRECTION('ref_axis',(0.,0.,-1.));
#15473=DIRECTION('center_axis',(8.96625347776458E-17,0.,1.));
#15474=DIRECTION('ref_axis',(1.,0.,0.));
#15475=DIRECTION('center_axis',(0.,-1.,0.));
#15476=DIRECTION('ref_axis',(0.,0.,-1.));
#15477=DIRECTION('center_axis',(0.,1.,0.));
#15478=DIRECTION('ref_axis',(1.,0.,0.));
#15479=DIRECTION('center_axis',(0.,-1.,0.));
#15480=DIRECTION('ref_axis',(1.,0.,0.));
#15481=DIRECTION('center_axis',(0.,-1.,0.));
#15482=DIRECTION('ref_axis',(0.,0.,-1.));
#15483=DIRECTION('center_axis',(0.,0.,1.));
#15484=DIRECTION('ref_axis',(1.,0.,0.));
#15485=DIRECTION('center_axis',(0.,-1.,0.));
#15486=DIRECTION('ref_axis',(0.,0.,-1.));
#15487=DIRECTION('center_axis',(0.,1.,0.));
#15488=DIRECTION('ref_axis',(1.,0.,0.));
#15489=DIRECTION('center_axis',(0.,-1.,0.));
#15490=DIRECTION('ref_axis',(1.,0.,0.));
#15491=DIRECTION('center_axis',(0.,-1.,0.));
#15492=DIRECTION('ref_axis',(1.,0.,0.));
#15493=DIRECTION('center_axis',(0.,-1.,0.));
#15494=DIRECTION('ref_axis',(0.,0.,-1.));
#15495=DIRECTION('center_axis',(0.,0.,1.));
#15496=DIRECTION('ref_axis',(1.,0.,0.));
#15497=DIRECTION('center_axis',(0.,-1.,0.));
#15498=DIRECTION('ref_axis',(0.,0.,-1.));
#15499=DIRECTION('center_axis',(0.,1.,0.));
#15500=DIRECTION('ref_axis',(1.,0.,0.));
#15501=DIRECTION('center_axis',(0.,-1.,0.));
#15502=DIRECTION('ref_axis',(1.,0.,0.));
#15503=DIRECTION('center_axis',(0.,-1.,0.));
#15504=DIRECTION('ref_axis',(0.,0.,-1.));
#15505=DIRECTION('center_axis',(8.96625347776458E-17,0.,1.));
#15506=DIRECTION('ref_axis',(1.,0.,0.));
#15507=DIRECTION('center_axis',(0.,-1.,0.));
#15508=DIRECTION('ref_axis',(0.,0.,-1.));
#15509=DIRECTION('center_axis',(0.,1.,0.));
#15510=DIRECTION('ref_axis',(1.,0.,0.));
#15511=DIRECTION('center_axis',(0.,-1.,0.));
#15512=DIRECTION('ref_axis',(1.,0.,0.));
#15513=DIRECTION('center_axis',(0.,-1.,0.));
#15514=DIRECTION('ref_axis',(0.,0.,-1.));
#15515=DIRECTION('center_axis',(0.,0.,1.));
#15516=DIRECTION('ref_axis',(1.,0.,0.));
#15517=DIRECTION('center_axis',(0.,-1.,0.));
#15518=DIRECTION('ref_axis',(0.,0.,-1.));
#15519=DIRECTION('center_axis',(0.,1.,0.));
#15520=DIRECTION('ref_axis',(1.,0.,0.));
#15521=DIRECTION('center_axis',(0.,1.,0.));
#15522=DIRECTION('ref_axis',(1.,0.,0.));
#15523=DIRECTION('',(0.,1.,0.));
#15524=DIRECTION('center_axis',(0.,-1.,0.));
#15525=DIRECTION('ref_axis',(1.,0.,0.));
#15526=DIRECTION('center_axis',(0.,-1.,0.));
#15527=DIRECTION('ref_axis',(1.,0.,0.));
#15528=DIRECTION('center_axis',(0.,1.,0.));
#15529=DIRECTION('ref_axis',(1.,0.,0.));
#15530=DIRECTION('center_axis',(0.,-1.,0.));
#15531=DIRECTION('ref_axis',(0.,0.,-1.));
#15532=DIRECTION('center_axis',(0.,0.,1.));
#15533=DIRECTION('ref_axis',(1.,0.,0.));
#15534=DIRECTION('center_axis',(0.,-1.,0.));
#15535=DIRECTION('ref_axis',(0.,0.,-1.));
#15536=DIRECTION('center_axis',(0.,-1.,0.));
#15537=DIRECTION('ref_axis',(-1.,0.,0.));
#15538=DIRECTION('center_axis',(0.,1.,0.));
#15539=DIRECTION('ref_axis',(1.,0.,0.));
#15540=DIRECTION('axis',(0.,0.,1.));
#15541=DIRECTION('refdir',(1.,0.,0.));
#15542=DIRECTION('center_axis',(0.,1.,0.));
#15543=DIRECTION('ref_axis',(0.,0.,1.));
#15544=DIRECTION('center_axis',(0.,-1.,0.));
#15545=DIRECTION('ref_axis',(1.,0.,0.));
#15546=DIRECTION('center_axis',(0.,-1.,0.));
#15547=DIRECTION('ref_axis',(1.,0.,0.));
#15548=DIRECTION('center_axis',(0.,-1.,0.));
#15549=DIRECTION('ref_axis',(1.,0.,0.));
#15550=DIRECTION('center_axis',(0.,-1.,0.));
#15551=DIRECTION('ref_axis',(1.,0.,0.));
#15552=DIRECTION('',(0.,1.,0.));
#15553=DIRECTION('center_axis',(0.,-1.,0.));
#15554=DIRECTION('ref_axis',(0.,0.,-1.));
#15555=DIRECTION('center_axis',(0.,-1.,0.));
#15556=DIRECTION('ref_axis',(1.,0.,0.));
#15557=DIRECTION('center_axis',(0.,-1.,0.));
#15558=DIRECTION('ref_axis',(1.,0.,0.));
#15559=DIRECTION('',(0.,1.,0.));
#15560=DIRECTION('center_axis',(0.,1.,0.));
#15561=DIRECTION('ref_axis',(0.,0.,1.));
#15562=DIRECTION('center_axis',(0.,-1.,0.));
#15563=DIRECTION('ref_axis',(1.,0.,0.));
#15564=DIRECTION('center_axis',(0.,-1.,0.));
#15565=DIRECTION('ref_axis',(1.,0.,0.));
#15566=DIRECTION('center_axis',(0.,-1.,0.));
#15567=DIRECTION('ref_axis',(1.,0.,0.));
#15568=DIRECTION('center_axis',(0.,-1.,0.));
#15569=DIRECTION('ref_axis',(1.,0.,0.));
#15570=DIRECTION('',(0.,1.,0.));
#15571=DIRECTION('center_axis',(0.,-1.,0.));
#15572=DIRECTION('ref_axis',(0.,0.,-1.));
#15573=DIRECTION('center_axis',(0.,-1.,0.));
#15574=DIRECTION('ref_axis',(1.,0.,0.));
#15575=DIRECTION('center_axis',(0.,-1.,0.));
#15576=DIRECTION('ref_axis',(1.,0.,0.));
#15577=DIRECTION('',(0.,1.,0.));
#15578=DIRECTION('',(0.,0.,1.));
#15579=DIRECTION('',(1.,0.,0.));
#15580=DIRECTION('',(0.,0.,1.));
#15581=DIRECTION('',(1.,0.,0.));
#15582=DIRECTION('',(0.,0.,1.));
#15583=DIRECTION('',(1.,0.,0.));
#15584=DIRECTION('',(0.,0.,1.));
#15585=DIRECTION('',(1.,0.,0.));
#15586=DIRECTION('',(0.,0.,1.));
#15587=DIRECTION('',(1.,0.,0.));
#15588=DIRECTION('axis',(0.,0.,1.));
#15589=DIRECTION('refdir',(1.,0.,0.));
#15590=DIRECTION('center_axis',(0.866025403784439,0.,-0.5));
#15591=DIRECTION('ref_axis',(0.5,0.,0.866025403784439));
#15592=DIRECTION('',(-0.5,0.,-0.866025403784439));
#15593=DIRECTION('',(0.,-1.,0.));
#15594=DIRECTION('',(0.5,0.,0.866025403784439));
#15595=DIRECTION('',(0.,-1.,0.));
#15596=DIRECTION('center_axis',(1.60246890531964E-16,0.,-1.));
#15597=DIRECTION('ref_axis',(1.,0.,1.60246890531964E-16));
#15598=DIRECTION('',(-1.,0.,-1.60246890531964E-16));
#15599=DIRECTION('',(0.,-1.,0.));
#15600=DIRECTION('',(1.,0.,1.60246890531964E-16));
#15601=DIRECTION('center_axis',(-0.866025403784439,0.,-0.5));
#15602=DIRECTION('ref_axis',(0.5,0.,-0.866025403784439));
#15603=DIRECTION('',(-0.5,0.,0.866025403784439));
#15604=DIRECTION('',(0.,-1.,0.));
#15605=DIRECTION('',(0.5,0.,-0.866025403784439));
#15606=DIRECTION('center_axis',(-0.866025403784439,0.,0.5));
#15607=DIRECTION('ref_axis',(-0.5,0.,-0.866025403784439));
#15608=DIRECTION('',(0.5,0.,0.866025403784439));
#15609=DIRECTION('',(0.,-1.,0.));
#15610=DIRECTION('',(-0.5,0.,-0.866025403784439));
#15611=DIRECTION('center_axis',(-1.60246890531964E-16,0.,1.));
#15612=DIRECTION('ref_axis',(-1.,0.,-1.60246890531964E-16));
#15613=DIRECTION('',(1.,0.,1.60246890531964E-16));
#15614=DIRECTION('',(0.,-1.,0.));
#15615=DIRECTION('',(-1.,0.,-1.60246890531964E-16));
#15616=DIRECTION('center_axis',(0.866025403784439,0.,0.5));
#15617=DIRECTION('ref_axis',(-0.5,0.,0.866025403784439));
#15618=DIRECTION('',(0.5,0.,-0.866025403784439));
#15619=DIRECTION('',(-0.5,0.,0.866025403784439));
#15620=DIRECTION('center_axis',(0.,1.,0.));
#15621=DIRECTION('ref_axis',(1.,0.,0.));
#15622=DIRECTION('center_axis',(0.,-1.,0.));
#15623=DIRECTION('ref_axis',(0.,0.,-1.));
#15624=DIRECTION('center_axis',(0.,1.,0.));
#15625=DIRECTION('ref_axis',(1.,0.,0.));
#15626=DIRECTION('center_axis',(0.,1.,0.));
#15627=DIRECTION('ref_axis',(1.,0.,0.));
#15628=DIRECTION('center_axis',(0.,1.,0.));
#15629=DIRECTION('ref_axis',(0.,0.,1.));
#15630=DIRECTION('center_axis',(0.,-1.,0.));
#15631=DIRECTION('ref_axis',(1.,0.,0.));
#15632=DIRECTION('center_axis',(0.,-1.,0.));
#15633=DIRECTION('ref_axis',(1.,0.,0.));
#15634=DIRECTION('center_axis',(0.,-1.,0.));
#15635=DIRECTION('ref_axis',(1.,0.,0.));
#15636=DIRECTION('',(0.707106781186547,0.707106781186548,8.65956056235493E-17));
#15637=DIRECTION('center_axis',(0.,-1.,0.));
#15638=DIRECTION('ref_axis',(1.,0.,0.));
#15639=DIRECTION('center_axis',(0.,-1.,0.));
#15640=DIRECTION('ref_axis',(1.,0.,0.));
#15641=DIRECTION('',(0.,1.,0.));
#15642=DIRECTION('center_axis',(0.,1.,0.));
#15643=DIRECTION('ref_axis',(1.,0.,0.));
#15644=DIRECTION('center_axis',(0.,-1.,0.));
#15645=DIRECTION('ref_axis',(1.,0.,0.));
#15646=DIRECTION('',(-0.707106781186547,0.707106781186548,-8.65956056235493E-17));
#15647=DIRECTION('center_axis',(0.,-1.,0.));
#15648=DIRECTION('ref_axis',(0.,0.,-1.));
#15649=DIRECTION('center_axis',(0.,-1.,0.));
#15650=DIRECTION('ref_axis',(1.,0.,0.));
#15651=DIRECTION('center_axis',(0.,1.,0.));
#15652=DIRECTION('ref_axis',(1.,0.,0.));
#15653=DIRECTION('center_axis',(0.,1.,0.));
#15654=DIRECTION('ref_axis',(1.,0.,0.));
#15655=DIRECTION('',(-0.447213595499958,0.894427190999916,-5.47678698264203E-17));
#15656=DIRECTION('center_axis',(0.,-1.,0.));
#15657=DIRECTION('ref_axis',(1.,0.,0.));
#15658=DIRECTION('',(0.,1.,0.));
#15659=DIRECTION('axis',(0.,0.,1.));
#15660=DIRECTION('refdir',(1.,0.,0.));
#15661=DIRECTION('axis',(0.,0.,1.));
#15662=DIRECTION('refdir',(1.,0.,0.));
#15663=DIRECTION('center_axis',(0.,0.,1.));
#15664=DIRECTION('ref_axis',(1.,0.,0.));
#15665=DIRECTION('center_axis',(0.,0.,1.));
#15666=DIRECTION('ref_axis',(1.,0.,0.));
#15667=DIRECTION('',(0.,0.,1.));
#15668=DIRECTION('center_axis',(0.,0.,1.));
#15669=DIRECTION('ref_axis',(1.,0.,0.));
#15670=DIRECTION('center_axis',(0.,0.,1.));
#15671=DIRECTION('ref_axis',(1.,0.,0.));
#15672=DIRECTION('center_axis',(1.,0.,0.));
#15673=DIRECTION('ref_axis',(0.,0.,-1.));
#15674=DIRECTION('',(0.,0.,-1.));
#15675=DIRECTION('',(0.,1.,0.));
#15676=DIRECTION('',(0.,0.,1.));
#15677=DIRECTION('',(0.,1.,0.));
#15678=DIRECTION('center_axis',(1.,0.,0.));
#15679=DIRECTION('ref_axis',(0.,0.,-1.));
#15680=DIRECTION('',(0.,0.,1.));
#15681=DIRECTION('',(0.,1.,0.));
#15682=DIRECTION('',(0.,0.,-1.));
#15683=DIRECTION('',(0.,1.,0.));
#15684=DIRECTION('center_axis',(0.,0.,-1.));
#15685=DIRECTION('ref_axis',(-1.,0.,0.));
#15686=DIRECTION('center_axis',(0.,0.,-1.));
#15687=DIRECTION('ref_axis',(1.,0.,0.));
#15688=DIRECTION('',(1.,0.,0.));
#15689=DIRECTION('',(0.,1.,0.));
#15690=DIRECTION('',(-1.,0.,0.));
#15691=DIRECTION('center_axis',(0.,0.,-1.));
#15692=DIRECTION('ref_axis',(1.,0.,0.));
#15693=DIRECTION('center_axis',(0.,0.,1.));
#15694=DIRECTION('ref_axis',(1.,0.,0.));
#15695=DIRECTION('center_axis',(0.,0.,1.));
#15696=DIRECTION('ref_axis',(1.,0.,0.));
#15697=DIRECTION('',(1.,0.,0.));
#15698=DIRECTION('',(0.,1.,0.));
#15699=DIRECTION('',(-1.,0.,0.));
#15700=DIRECTION('center_axis',(0.,0.,1.));
#15701=DIRECTION('ref_axis',(1.,0.,0.));
#15702=DIRECTION('center_axis',(-1.,0.,0.));
#15703=DIRECTION('ref_axis',(0.,0.,1.));
#15704=DIRECTION('',(0.,0.,-1.));
#15705=DIRECTION('',(0.,0.,1.));
#15706=DIRECTION('',(0.,1.,0.));
#15707=DIRECTION('center_axis',(-0.342020143325675,0.,0.939692620785906));
#15708=DIRECTION('ref_axis',(0.939692620785906,0.,0.342020143325675));
#15709=DIRECTION('',(-0.939692620785906,0.,-0.342020143325675));
#15710=DIRECTION('',(0.939692620785906,0.,0.342020143325675));
#15711=DIRECTION('',(0.,1.,0.));
#15712=DIRECTION('center_axis',(-1.,0.,0.));
#15713=DIRECTION('ref_axis',(0.,0.,1.));
#15714=DIRECTION('',(0.,0.,-1.));
#15715=DIRECTION('',(0.,0.,1.));
#15716=DIRECTION('',(0.,1.,0.));
#15717=DIRECTION('center_axis',(-0.342020143325675,0.,-0.939692620785906));
#15718=DIRECTION('ref_axis',(-0.939692620785906,0.,0.342020143325675));
#15719=DIRECTION('',(0.939692620785906,0.,-0.342020143325675));
#15720=DIRECTION('',(-0.939692620785906,0.,0.342020143325675));
#15721=DIRECTION('',(0.,1.,0.));
#15722=DIRECTION('center_axis',(-1.,0.,0.));
#15723=DIRECTION('ref_axis',(0.,0.,1.));
#15724=DIRECTION('',(0.,0.,-1.));
#15725=DIRECTION('',(0.,0.,1.));
#15726=DIRECTION('',(0.,1.,0.));
#15727=DIRECTION('center_axis',(-0.342020143325675,0.,0.939692620785906));
#15728=DIRECTION('ref_axis',(0.939692620785906,0.,0.342020143325675));
#15729=DIRECTION('',(-0.939692620785906,0.,-0.342020143325675));
#15730=DIRECTION('',(0.939692620785906,0.,0.342020143325675));
#15731=DIRECTION('',(0.,1.,0.));
#15732=DIRECTION('center_axis',(-1.,0.,0.));
#15733=DIRECTION('ref_axis',(0.,0.,1.));
#15734=DIRECTION('',(0.,0.,-1.));
#15735=DIRECTION('',(0.,0.,1.));
#15736=DIRECTION('',(0.,1.,0.));
#15737=DIRECTION('center_axis',(-0.342020143325675,0.,-0.939692620785906));
#15738=DIRECTION('ref_axis',(-0.939692620785906,0.,0.342020143325675));
#15739=DIRECTION('',(0.939692620785906,0.,-0.342020143325675));
#15740=DIRECTION('',(-0.939692620785906,0.,0.342020143325675));
#15741=DIRECTION('',(0.,1.,0.));
#15742=DIRECTION('center_axis',(-1.,0.,0.));
#15743=DIRECTION('ref_axis',(0.,0.,1.));
#15744=DIRECTION('',(0.,0.,-1.));
#15745=DIRECTION('',(0.,0.,1.));
#15746=DIRECTION('',(0.,1.,0.));
#15747=DIRECTION('center_axis',(-0.342020143325675,0.,0.939692620785906));
#15748=DIRECTION('ref_axis',(0.939692620785906,0.,0.342020143325675));
#15749=DIRECTION('',(-0.939692620785906,0.,-0.342020143325675));
#15750=DIRECTION('',(0.939692620785906,0.,0.342020143325675));
#15751=DIRECTION('',(0.,1.,0.));
#15752=DIRECTION('center_axis',(-1.,0.,0.));
#15753=DIRECTION('ref_axis',(0.,0.,1.));
#15754=DIRECTION('',(0.,0.,-1.));
#15755=DIRECTION('',(0.,0.,1.));
#15756=DIRECTION('',(0.,1.,0.));
#15757=DIRECTION('center_axis',(-0.342020143325675,0.,-0.939692620785906));
#15758=DIRECTION('ref_axis',(-0.939692620785906,0.,0.342020143325675));
#15759=DIRECTION('',(0.939692620785906,0.,-0.342020143325675));
#15760=DIRECTION('',(-0.939692620785906,0.,0.342020143325675));
#15761=DIRECTION('',(0.,1.,0.));
#15762=DIRECTION('center_axis',(-1.,0.,0.));
#15763=DIRECTION('ref_axis',(0.,0.,1.));
#15764=DIRECTION('',(0.,0.,-1.));
#15765=DIRECTION('',(0.,0.,1.));
#15766=DIRECTION('',(0.,1.,0.));
#15767=DIRECTION('center_axis',(-0.342020143325675,0.,0.939692620785906));
#15768=DIRECTION('ref_axis',(0.939692620785906,0.,0.342020143325675));
#15769=DIRECTION('',(-0.939692620785906,0.,-0.342020143325675));
#15770=DIRECTION('',(0.939692620785906,0.,0.342020143325675));
#15771=DIRECTION('',(0.,1.,0.));
#15772=DIRECTION('center_axis',(-1.,0.,0.));
#15773=DIRECTION('ref_axis',(0.,0.,1.));
#15774=DIRECTION('',(0.,0.,-1.));
#15775=DIRECTION('',(0.,0.,1.));
#15776=DIRECTION('',(0.,1.,0.));
#15777=DIRECTION('center_axis',(-0.342020143325675,0.,-0.939692620785906));
#15778=DIRECTION('ref_axis',(-0.939692620785906,0.,0.342020143325675));
#15779=DIRECTION('',(0.939692620785906,0.,-0.342020143325675));
#15780=DIRECTION('',(-0.939692620785906,0.,0.342020143325675));
#15781=DIRECTION('',(0.,1.,0.));
#15782=DIRECTION('center_axis',(-1.,0.,0.));
#15783=DIRECTION('ref_axis',(0.,0.,1.));
#15784=DIRECTION('',(0.,0.,-1.));
#15785=DIRECTION('',(0.,0.,1.));
#15786=DIRECTION('',(0.,1.,0.));
#15787=DIRECTION('center_axis',(-0.342020143325662,0.,0.939692620785911));
#15788=DIRECTION('ref_axis',(0.939692620785911,0.,0.342020143325662));
#15789=DIRECTION('',(-0.939692620785911,0.,-0.342020143325662));
#15790=DIRECTION('',(0.939692620785911,0.,0.342020143325662));
#15791=DIRECTION('',(0.,1.,0.));
#15792=DIRECTION('center_axis',(-1.,0.,0.));
#15793=DIRECTION('ref_axis',(0.,0.,1.));
#15794=DIRECTION('',(0.,0.,-1.));
#15795=DIRECTION('',(0.,0.,1.));
#15796=DIRECTION('',(0.,1.,0.));
#15797=DIRECTION('center_axis',(-0.342020143325662,0.,-0.939692620785911));
#15798=DIRECTION('ref_axis',(-0.939692620785911,0.,0.342020143325662));
#15799=DIRECTION('',(0.939692620785911,0.,-0.342020143325662));
#15800=DIRECTION('',(-0.939692620785911,0.,0.342020143325662));
#15801=DIRECTION('',(0.,1.,0.));
#15802=DIRECTION('center_axis',(-1.,0.,0.));
#15803=DIRECTION('ref_axis',(0.,0.,1.));
#15804=DIRECTION('',(0.,0.,-1.));
#15805=DIRECTION('',(0.,0.,1.));
#15806=DIRECTION('',(0.,1.,0.));
#15807=DIRECTION('center_axis',(-0.342020143325662,0.,0.939692620785911));
#15808=DIRECTION('ref_axis',(0.939692620785911,0.,0.342020143325662));
#15809=DIRECTION('',(-0.939692620785911,0.,-0.342020143325662));
#15810=DIRECTION('',(0.939692620785911,0.,0.342020143325662));
#15811=DIRECTION('',(0.,1.,0.));
#15812=DIRECTION('center_axis',(-1.,0.,0.));
#15813=DIRECTION('ref_axis',(0.,0.,1.));
#15814=DIRECTION('',(0.,0.,-1.));
#15815=DIRECTION('',(0.,0.,1.));
#15816=DIRECTION('',(0.,1.,0.));
#15817=DIRECTION('center_axis',(-0.342020143325662,0.,-0.939692620785911));
#15818=DIRECTION('ref_axis',(-0.939692620785911,0.,0.342020143325662));
#15819=DIRECTION('',(0.939692620785911,0.,-0.342020143325662));
#15820=DIRECTION('',(-0.939692620785911,0.,0.342020143325662));
#15821=DIRECTION('',(0.,1.,0.));
#15822=DIRECTION('center_axis',(-1.,0.,0.));
#15823=DIRECTION('ref_axis',(0.,0.,1.));
#15824=DIRECTION('',(0.,0.,-1.));
#15825=DIRECTION('',(0.,0.,1.));
#15826=DIRECTION('',(0.,1.,0.));
#15827=DIRECTION('center_axis',(-0.342020143325662,0.,0.939692620785911));
#15828=DIRECTION('ref_axis',(0.939692620785911,0.,0.342020143325662));
#15829=DIRECTION('',(-0.939692620785911,0.,-0.342020143325662));
#15830=DIRECTION('',(0.939692620785911,0.,0.342020143325662));
#15831=DIRECTION('',(0.,1.,0.));
#15832=DIRECTION('center_axis',(-1.,0.,0.));
#15833=DIRECTION('ref_axis',(0.,0.,1.));
#15834=DIRECTION('',(0.,0.,-1.));
#15835=DIRECTION('',(0.,0.,1.));
#15836=DIRECTION('',(0.,1.,0.));
#15837=DIRECTION('center_axis',(-0.342020143325662,0.,-0.939692620785911));
#15838=DIRECTION('ref_axis',(-0.939692620785911,0.,0.342020143325662));
#15839=DIRECTION('',(0.939692620785911,0.,-0.342020143325662));
#15840=DIRECTION('',(-0.939692620785911,0.,0.342020143325662));
#15841=DIRECTION('',(0.,1.,0.));
#15842=DIRECTION('center_axis',(-1.,0.,0.));
#15843=DIRECTION('ref_axis',(0.,0.,1.));
#15844=DIRECTION('',(0.,0.,-1.));
#15845=DIRECTION('',(0.,0.,1.));
#15846=DIRECTION('',(0.,1.,0.));
#15847=DIRECTION('center_axis',(-0.342020143325668,0.,0.939692620785909));
#15848=DIRECTION('ref_axis',(0.939692620785909,0.,0.342020143325668));
#15849=DIRECTION('',(-0.939692620785909,0.,-0.342020143325668));
#15850=DIRECTION('',(0.939692620785909,0.,0.342020143325668));
#15851=DIRECTION('',(0.,1.,0.));
#15852=DIRECTION('center_axis',(-1.,0.,0.));
#15853=DIRECTION('ref_axis',(0.,0.,1.));
#15854=DIRECTION('',(0.,0.,-1.));
#15855=DIRECTION('',(0.,0.,1.));
#15856=DIRECTION('',(0.,1.,0.));
#15857=DIRECTION('center_axis',(-0.342020143325668,0.,-0.939692620785909));
#15858=DIRECTION('ref_axis',(-0.939692620785909,0.,0.342020143325668));
#15859=DIRECTION('',(0.939692620785909,0.,-0.342020143325668));
#15860=DIRECTION('',(-0.939692620785909,0.,0.342020143325668));
#15861=DIRECTION('',(0.,1.,0.));
#15862=DIRECTION('center_axis',(-1.,0.,0.));
#15863=DIRECTION('ref_axis',(0.,0.,1.));
#15864=DIRECTION('',(0.,0.,-1.));
#15865=DIRECTION('',(0.,0.,1.));
#15866=DIRECTION('',(0.,1.,0.));
#15867=DIRECTION('center_axis',(-0.342020143325668,0.,0.939692620785909));
#15868=DIRECTION('ref_axis',(0.939692620785909,0.,0.342020143325668));
#15869=DIRECTION('',(-0.939692620785909,0.,-0.342020143325668));
#15870=DIRECTION('',(0.939692620785909,0.,0.342020143325668));
#15871=DIRECTION('',(0.,1.,0.));
#15872=DIRECTION('center_axis',(-1.,0.,0.));
#15873=DIRECTION('ref_axis',(0.,0.,1.));
#15874=DIRECTION('',(0.,0.,-1.));
#15875=DIRECTION('',(0.,0.,1.));
#15876=DIRECTION('',(0.,1.,0.));
#15877=DIRECTION('center_axis',(-0.342020143325668,0.,-0.939692620785909));
#15878=DIRECTION('ref_axis',(-0.939692620785909,0.,0.342020143325668));
#15879=DIRECTION('',(0.939692620785909,0.,-0.342020143325668));
#15880=DIRECTION('',(-0.939692620785909,0.,0.342020143325668));
#15881=DIRECTION('',(0.,1.,0.));
#15882=DIRECTION('center_axis',(-1.,0.,0.));
#15883=DIRECTION('ref_axis',(0.,0.,1.));
#15884=DIRECTION('',(0.,0.,-1.));
#15885=DIRECTION('',(0.,0.,1.));
#15886=DIRECTION('',(0.,1.,0.));
#15887=DIRECTION('center_axis',(-0.342020143325668,0.,0.939692620785909));
#15888=DIRECTION('ref_axis',(0.939692620785909,0.,0.342020143325668));
#15889=DIRECTION('',(-0.939692620785909,0.,-0.342020143325668));
#15890=DIRECTION('',(0.939692620785909,0.,0.342020143325668));
#15891=DIRECTION('',(0.,1.,0.));
#15892=DIRECTION('center_axis',(-1.,0.,0.));
#15893=DIRECTION('ref_axis',(0.,0.,1.));
#15894=DIRECTION('',(0.,0.,-1.));
#15895=DIRECTION('',(0.,0.,1.));
#15896=DIRECTION('',(0.,1.,0.));
#15897=DIRECTION('center_axis',(-0.342020143325668,0.,-0.939692620785909));
#15898=DIRECTION('ref_axis',(-0.939692620785909,0.,0.342020143325668));
#15899=DIRECTION('',(0.939692620785909,0.,-0.342020143325668));
#15900=DIRECTION('',(-0.939692620785909,0.,0.342020143325668));
#15901=DIRECTION('',(0.,1.,0.));
#15902=DIRECTION('center_axis',(-1.,0.,0.));
#15903=DIRECTION('ref_axis',(0.,0.,1.));
#15904=DIRECTION('',(0.,0.,-1.));
#15905=DIRECTION('',(0.,0.,1.));
#15906=DIRECTION('',(0.,1.,0.));
#15907=DIRECTION('center_axis',(-0.342020143325668,0.,0.939692620785909));
#15908=DIRECTION('ref_axis',(0.939692620785909,0.,0.342020143325668));
#15909=DIRECTION('',(-0.939692620785909,0.,-0.342020143325668));
#15910=DIRECTION('',(0.939692620785909,0.,0.342020143325668));
#15911=DIRECTION('',(0.,1.,0.));
#15912=DIRECTION('center_axis',(-1.,0.,0.));
#15913=DIRECTION('ref_axis',(0.,0.,1.));
#15914=DIRECTION('',(0.,0.,-1.));
#15915=DIRECTION('',(0.,0.,1.));
#15916=DIRECTION('',(0.,1.,0.));
#15917=DIRECTION('center_axis',(-0.342020143325668,0.,-0.939692620785909));
#15918=DIRECTION('ref_axis',(-0.939692620785909,0.,0.342020143325668));
#15919=DIRECTION('',(0.939692620785909,0.,-0.342020143325668));
#15920=DIRECTION('',(-0.939692620785909,0.,0.342020143325668));
#15921=DIRECTION('',(0.,1.,0.));
#15922=DIRECTION('center_axis',(-1.,0.,0.));
#15923=DIRECTION('ref_axis',(0.,0.,1.));
#15924=DIRECTION('',(0.,0.,-1.));
#15925=DIRECTION('',(0.,0.,1.));
#15926=DIRECTION('',(0.,1.,0.));
#15927=DIRECTION('center_axis',(-0.342020143325668,0.,0.939692620785909));
#15928=DIRECTION('ref_axis',(0.939692620785909,0.,0.342020143325668));
#15929=DIRECTION('',(-0.939692620785909,0.,-0.342020143325668));
#15930=DIRECTION('',(0.939692620785909,0.,0.342020143325668));
#15931=DIRECTION('',(0.,1.,0.));
#15932=DIRECTION('center_axis',(-1.,0.,0.));
#15933=DIRECTION('ref_axis',(0.,0.,1.));
#15934=DIRECTION('',(0.,0.,-1.));
#15935=DIRECTION('',(0.,0.,1.));
#15936=DIRECTION('',(0.,1.,0.));
#15937=DIRECTION('center_axis',(-0.342020143325668,0.,-0.939692620785909));
#15938=DIRECTION('ref_axis',(-0.939692620785909,0.,0.342020143325668));
#15939=DIRECTION('',(0.939692620785909,0.,-0.342020143325668));
#15940=DIRECTION('',(-0.939692620785909,0.,0.342020143325668));
#15941=DIRECTION('',(0.,1.,0.));
#15942=DIRECTION('center_axis',(-1.,0.,0.));
#15943=DIRECTION('ref_axis',(0.,0.,1.));
#15944=DIRECTION('',(0.,0.,-1.));
#15945=DIRECTION('',(0.,0.,1.));
#15946=DIRECTION('',(0.,1.,0.));
#15947=DIRECTION('center_axis',(-0.342020143325668,0.,0.939692620785909));
#15948=DIRECTION('ref_axis',(0.939692620785909,0.,0.342020143325668));
#15949=DIRECTION('',(-0.939692620785909,0.,-0.342020143325668));
#15950=DIRECTION('',(0.939692620785909,0.,0.342020143325668));
#15951=DIRECTION('',(0.,1.,0.));
#15952=DIRECTION('center_axis',(-1.,0.,0.));
#15953=DIRECTION('ref_axis',(0.,0.,1.));
#15954=DIRECTION('',(0.,0.,-1.));
#15955=DIRECTION('',(0.,0.,1.));
#15956=DIRECTION('',(0.,1.,0.));
#15957=DIRECTION('center_axis',(-0.342020143325668,0.,-0.939692620785909));
#15958=DIRECTION('ref_axis',(-0.939692620785909,0.,0.342020143325668));
#15959=DIRECTION('',(0.939692620785909,0.,-0.342020143325668));
#15960=DIRECTION('',(-0.939692620785909,0.,0.342020143325668));
#15961=DIRECTION('',(0.,1.,0.));
#15962=DIRECTION('center_axis',(-1.,0.,0.));
#15963=DIRECTION('ref_axis',(0.,0.,1.));
#15964=DIRECTION('',(0.,0.,-1.));
#15965=DIRECTION('',(0.,0.,1.));
#15966=DIRECTION('',(0.,1.,0.));
#15967=DIRECTION('center_axis',(-0.342020143325668,0.,0.939692620785909));
#15968=DIRECTION('ref_axis',(0.939692620785909,0.,0.342020143325668));
#15969=DIRECTION('',(-0.939692620785909,0.,-0.342020143325668));
#15970=DIRECTION('',(0.939692620785909,0.,0.342020143325668));
#15971=DIRECTION('',(0.,1.,0.));
#15972=DIRECTION('center_axis',(-1.,0.,0.));
#15973=DIRECTION('ref_axis',(0.,0.,1.));
#15974=DIRECTION('',(0.,0.,-1.));
#15975=DIRECTION('',(0.,0.,1.));
#15976=DIRECTION('',(0.,1.,0.));
#15977=DIRECTION('center_axis',(-0.342020143325668,0.,-0.939692620785909));
#15978=DIRECTION('ref_axis',(-0.939692620785909,0.,0.342020143325668));
#15979=DIRECTION('',(0.939692620785909,0.,-0.342020143325668));
#15980=DIRECTION('',(-0.939692620785909,0.,0.342020143325668));
#15981=DIRECTION('',(0.,1.,0.));
#15982=DIRECTION('center_axis',(-1.,0.,0.));
#15983=DIRECTION('ref_axis',(0.,0.,1.));
#15984=DIRECTION('',(0.,0.,-1.));
#15985=DIRECTION('',(0.,0.,1.));
#15986=DIRECTION('',(0.,1.,0.));
#15987=DIRECTION('center_axis',(-0.342020143325662,0.,0.939692620785911));
#15988=DIRECTION('ref_axis',(0.939692620785911,0.,0.342020143325662));
#15989=DIRECTION('',(-0.939692620785911,0.,-0.342020143325662));
#15990=DIRECTION('',(0.939692620785911,0.,0.342020143325662));
#15991=DIRECTION('',(0.,1.,0.));
#15992=DIRECTION('center_axis',(-1.,0.,0.));
#15993=DIRECTION('ref_axis',(0.,0.,1.));
#15994=DIRECTION('',(0.,0.,-1.));
#15995=DIRECTION('',(0.,0.,1.));
#15996=DIRECTION('',(0.,1.,0.));
#15997=DIRECTION('center_axis',(-0.342020143325662,0.,-0.939692620785911));
#15998=DIRECTION('ref_axis',(-0.939692620785911,0.,0.342020143325662));
#15999=DIRECTION('',(0.939692620785911,0.,-0.342020143325662));
#16000=DIRECTION('',(-0.939692620785911,0.,0.342020143325662));
#16001=DIRECTION('',(0.,1.,0.));
#16002=DIRECTION('center_axis',(-1.,0.,0.));
#16003=DIRECTION('ref_axis',(0.,0.,1.));
#16004=DIRECTION('',(0.,0.,-1.));
#16005=DIRECTION('',(0.,0.,1.));
#16006=DIRECTION('',(0.,1.,0.));
#16007=DIRECTION('center_axis',(-0.342020143325668,0.,0.939692620785909));
#16008=DIRECTION('ref_axis',(0.939692620785909,0.,0.342020143325668));
#16009=DIRECTION('',(-0.939692620785909,0.,-0.342020143325668));
#16010=DIRECTION('',(0.939692620785909,0.,0.342020143325668));
#16011=DIRECTION('',(0.,1.,0.));
#16012=DIRECTION('center_axis',(-1.,0.,0.));
#16013=DIRECTION('ref_axis',(0.,0.,1.));
#16014=DIRECTION('',(0.,0.,-1.));
#16015=DIRECTION('',(0.,0.,1.));
#16016=DIRECTION('',(0.,1.,0.));
#16017=DIRECTION('center_axis',(-0.342020143325668,0.,-0.939692620785909));
#16018=DIRECTION('ref_axis',(-0.939692620785909,0.,0.342020143325668));
#16019=DIRECTION('',(0.939692620785909,0.,-0.342020143325668));
#16020=DIRECTION('',(-0.939692620785909,0.,0.342020143325668));
#16021=DIRECTION('',(0.,1.,0.));
#16022=DIRECTION('center_axis',(-1.,0.,0.));
#16023=DIRECTION('ref_axis',(0.,0.,1.));
#16024=DIRECTION('',(0.,0.,-1.));
#16025=DIRECTION('',(0.,0.,1.));
#16026=DIRECTION('',(0.,1.,0.));
#16027=DIRECTION('center_axis',(-0.342020143325668,0.,0.939692620785909));
#16028=DIRECTION('ref_axis',(0.939692620785909,0.,0.342020143325668));
#16029=DIRECTION('',(-0.939692620785909,0.,-0.342020143325668));
#16030=DIRECTION('',(0.939692620785909,0.,0.342020143325668));
#16031=DIRECTION('',(0.,1.,0.));
#16032=DIRECTION('center_axis',(-1.,0.,0.));
#16033=DIRECTION('ref_axis',(0.,0.,1.));
#16034=DIRECTION('',(0.,0.,-1.));
#16035=DIRECTION('',(0.,0.,1.));
#16036=DIRECTION('',(0.,1.,0.));
#16037=DIRECTION('center_axis',(-0.342020143325668,0.,-0.939692620785909));
#16038=DIRECTION('ref_axis',(-0.939692620785909,0.,0.342020143325668));
#16039=DIRECTION('',(0.939692620785909,0.,-0.342020143325668));
#16040=DIRECTION('',(-0.939692620785909,0.,0.342020143325668));
#16041=DIRECTION('',(0.,1.,0.));
#16042=DIRECTION('center_axis',(-1.,0.,0.));
#16043=DIRECTION('ref_axis',(0.,0.,1.));
#16044=DIRECTION('',(0.,0.,-1.));
#16045=DIRECTION('',(0.,0.,1.));
#16046=DIRECTION('',(0.,1.,0.));
#16047=DIRECTION('center_axis',(-0.342020143325668,0.,0.939692620785909));
#16048=DIRECTION('ref_axis',(0.939692620785909,0.,0.342020143325668));
#16049=DIRECTION('',(-0.939692620785909,0.,-0.342020143325668));
#16050=DIRECTION('',(0.939692620785909,0.,0.342020143325668));
#16051=DIRECTION('',(0.,1.,0.));
#16052=DIRECTION('center_axis',(-1.,0.,0.));
#16053=DIRECTION('ref_axis',(0.,0.,1.));
#16054=DIRECTION('',(0.,0.,-1.));
#16055=DIRECTION('',(0.,0.,1.));
#16056=DIRECTION('',(0.,1.,0.));
#16057=DIRECTION('center_axis',(-0.342020143325662,0.,-0.939692620785911));
#16058=DIRECTION('ref_axis',(-0.939692620785911,0.,0.342020143325662));
#16059=DIRECTION('',(0.939692620785911,0.,-0.342020143325662));
#16060=DIRECTION('',(-0.939692620785911,0.,0.342020143325662));
#16061=DIRECTION('',(0.,1.,0.));
#16062=DIRECTION('center_axis',(-1.,0.,0.));
#16063=DIRECTION('ref_axis',(0.,0.,1.));
#16064=DIRECTION('',(0.,0.,-1.));
#16065=DIRECTION('',(0.,0.,1.));
#16066=DIRECTION('',(0.,1.,0.));
#16067=DIRECTION('center_axis',(-0.342020143325668,0.,0.939692620785909));
#16068=DIRECTION('ref_axis',(0.939692620785909,0.,0.342020143325668));
#16069=DIRECTION('',(-0.939692620785909,0.,-0.342020143325668));
#16070=DIRECTION('',(0.939692620785909,0.,0.342020143325668));
#16071=DIRECTION('',(0.,1.,0.));
#16072=DIRECTION('center_axis',(-1.,0.,0.));
#16073=DIRECTION('ref_axis',(0.,0.,1.));
#16074=DIRECTION('',(0.,0.,-1.));
#16075=DIRECTION('',(0.,0.,1.));
#16076=DIRECTION('',(0.,1.,0.));
#16077=DIRECTION('center_axis',(-0.342020143325668,0.,-0.939692620785909));
#16078=DIRECTION('ref_axis',(-0.939692620785909,0.,0.342020143325668));
#16079=DIRECTION('',(0.939692620785909,0.,-0.342020143325668));
#16080=DIRECTION('',(-0.939692620785909,0.,0.342020143325668));
#16081=DIRECTION('',(0.,1.,0.));
#16082=DIRECTION('center_axis',(-1.,0.,0.));
#16083=DIRECTION('ref_axis',(0.,0.,1.));
#16084=DIRECTION('',(0.,0.,-1.));
#16085=DIRECTION('',(0.,0.,1.));
#16086=DIRECTION('',(0.,1.,0.));
#16087=DIRECTION('center_axis',(-0.342020143325662,0.,0.939692620785911));
#16088=DIRECTION('ref_axis',(0.939692620785911,0.,0.342020143325662));
#16089=DIRECTION('',(-0.939692620785911,0.,-0.342020143325662));
#16090=DIRECTION('',(0.939692620785911,0.,0.342020143325662));
#16091=DIRECTION('',(0.,1.,0.));
#16092=DIRECTION('center_axis',(-1.,0.,0.));
#16093=DIRECTION('ref_axis',(0.,0.,1.));
#16094=DIRECTION('',(0.,0.,-1.));
#16095=DIRECTION('',(0.,0.,1.));
#16096=DIRECTION('',(0.,1.,0.));
#16097=DIRECTION('center_axis',(-0.342020143325668,0.,-0.939692620785909));
#16098=DIRECTION('ref_axis',(-0.939692620785909,0.,0.342020143325668));
#16099=DIRECTION('',(0.939692620785909,0.,-0.342020143325668));
#16100=DIRECTION('',(-0.939692620785909,0.,0.342020143325668));
#16101=DIRECTION('',(0.,1.,0.));
#16102=DIRECTION('center_axis',(-1.,0.,0.));
#16103=DIRECTION('ref_axis',(0.,0.,1.));
#16104=DIRECTION('',(0.,0.,-1.));
#16105=DIRECTION('',(0.,0.,1.));
#16106=DIRECTION('',(0.,1.,0.));
#16107=DIRECTION('center_axis',(-0.342020143325668,0.,0.939692620785909));
#16108=DIRECTION('ref_axis',(0.939692620785909,0.,0.342020143325668));
#16109=DIRECTION('',(-0.939692620785909,0.,-0.342020143325668));
#16110=DIRECTION('',(0.939692620785909,0.,0.342020143325668));
#16111=DIRECTION('',(0.,1.,0.));
#16112=DIRECTION('center_axis',(-1.,0.,0.));
#16113=DIRECTION('ref_axis',(0.,0.,1.));
#16114=DIRECTION('',(0.,0.,-1.));
#16115=DIRECTION('',(0.,0.,1.));
#16116=DIRECTION('',(0.,1.,0.));
#16117=DIRECTION('center_axis',(-0.342020143325668,0.,-0.939692620785909));
#16118=DIRECTION('ref_axis',(-0.939692620785909,0.,0.342020143325668));
#16119=DIRECTION('',(0.939692620785909,0.,-0.342020143325668));
#16120=DIRECTION('',(-0.939692620785909,0.,0.342020143325668));
#16121=DIRECTION('',(0.,1.,0.));
#16122=DIRECTION('center_axis',(-1.,0.,0.));
#16123=DIRECTION('ref_axis',(0.,0.,1.));
#16124=DIRECTION('',(0.,0.,-1.));
#16125=DIRECTION('',(0.,0.,1.));
#16126=DIRECTION('',(0.,1.,0.));
#16127=DIRECTION('center_axis',(-0.342020143325668,0.,0.939692620785909));
#16128=DIRECTION('ref_axis',(0.939692620785909,0.,0.342020143325668));
#16129=DIRECTION('',(-0.939692620785909,0.,-0.342020143325668));
#16130=DIRECTION('',(0.939692620785909,0.,0.342020143325668));
#16131=DIRECTION('',(0.,1.,0.));
#16132=DIRECTION('center_axis',(-1.,0.,0.));
#16133=DIRECTION('ref_axis',(0.,0.,1.));
#16134=DIRECTION('',(0.,0.,-1.));
#16135=DIRECTION('',(0.,0.,1.));
#16136=DIRECTION('',(0.,1.,0.));
#16137=DIRECTION('center_axis',(-0.342020143325662,0.,-0.939692620785911));
#16138=DIRECTION('ref_axis',(-0.939692620785911,0.,0.342020143325662));
#16139=DIRECTION('',(0.939692620785911,0.,-0.342020143325662));
#16140=DIRECTION('',(-0.939692620785911,0.,0.342020143325662));
#16141=DIRECTION('',(0.,1.,0.));
#16142=DIRECTION('center_axis',(-1.,0.,0.));
#16143=DIRECTION('ref_axis',(0.,0.,1.));
#16144=DIRECTION('',(0.,0.,-1.));
#16145=DIRECTION('',(0.,0.,1.));
#16146=DIRECTION('',(0.,1.,0.));
#16147=DIRECTION('center_axis',(-0.342020143325668,0.,0.939692620785909));
#16148=DIRECTION('ref_axis',(0.939692620785909,0.,0.342020143325668));
#16149=DIRECTION('',(-0.939692620785909,0.,-0.342020143325668));
#16150=DIRECTION('',(0.939692620785909,0.,0.342020143325668));
#16151=DIRECTION('',(0.,1.,0.));
#16152=DIRECTION('center_axis',(-1.,0.,0.));
#16153=DIRECTION('ref_axis',(0.,0.,1.));
#16154=DIRECTION('',(0.,0.,-1.));
#16155=DIRECTION('',(0.,0.,1.));
#16156=DIRECTION('',(0.,1.,0.));
#16157=DIRECTION('center_axis',(-0.342020143325668,0.,-0.939692620785909));
#16158=DIRECTION('ref_axis',(-0.939692620785909,0.,0.342020143325668));
#16159=DIRECTION('',(0.939692620785909,0.,-0.342020143325668));
#16160=DIRECTION('',(-0.939692620785909,0.,0.342020143325668));
#16161=DIRECTION('',(0.,1.,0.));
#16162=DIRECTION('center_axis',(-1.,0.,0.));
#16163=DIRECTION('ref_axis',(0.,0.,1.));
#16164=DIRECTION('',(0.,0.,-1.));
#16165=DIRECTION('',(0.,0.,1.));
#16166=DIRECTION('',(0.,1.,0.));
#16167=DIRECTION('center_axis',(-0.342020143325668,0.,0.939692620785909));
#16168=DIRECTION('ref_axis',(0.939692620785909,0.,0.342020143325668));
#16169=DIRECTION('',(-0.939692620785909,0.,-0.342020143325668));
#16170=DIRECTION('',(0.939692620785909,0.,0.342020143325668));
#16171=DIRECTION('',(0.,1.,0.));
#16172=DIRECTION('center_axis',(-1.,0.,0.));
#16173=DIRECTION('ref_axis',(0.,0.,1.));
#16174=DIRECTION('',(0.,0.,-1.));
#16175=DIRECTION('',(0.,0.,1.));
#16176=DIRECTION('',(0.,1.,0.));
#16177=DIRECTION('center_axis',(-0.342020143325668,0.,-0.939692620785909));
#16178=DIRECTION('ref_axis',(-0.939692620785909,0.,0.342020143325668));
#16179=DIRECTION('',(0.939692620785909,0.,-0.342020143325668));
#16180=DIRECTION('',(-0.939692620785909,0.,0.342020143325668));
#16181=DIRECTION('',(0.,1.,0.));
#16182=DIRECTION('center_axis',(-1.,0.,0.));
#16183=DIRECTION('ref_axis',(0.,0.,1.));
#16184=DIRECTION('',(0.,0.,-1.));
#16185=DIRECTION('',(0.,0.,1.));
#16186=DIRECTION('',(0.,1.,0.));
#16187=DIRECTION('center_axis',(-0.342020143325668,0.,0.939692620785909));
#16188=DIRECTION('ref_axis',(0.939692620785909,0.,0.342020143325668));
#16189=DIRECTION('',(-0.939692620785909,0.,-0.342020143325668));
#16190=DIRECTION('',(0.939692620785909,0.,0.342020143325668));
#16191=DIRECTION('',(0.,1.,0.));
#16192=DIRECTION('center_axis',(-1.,0.,0.));
#16193=DIRECTION('ref_axis',(0.,0.,1.));
#16194=DIRECTION('',(0.,0.,-1.));
#16195=DIRECTION('',(0.,0.,1.));
#16196=DIRECTION('',(0.,1.,0.));
#16197=DIRECTION('center_axis',(-0.342020143325668,0.,-0.939692620785909));
#16198=DIRECTION('ref_axis',(-0.939692620785909,0.,0.342020143325668));
#16199=DIRECTION('',(0.939692620785909,0.,-0.342020143325668));
#16200=DIRECTION('',(-0.939692620785909,0.,0.342020143325668));
#16201=DIRECTION('',(0.,1.,0.));
#16202=DIRECTION('center_axis',(-1.,0.,0.));
#16203=DIRECTION('ref_axis',(0.,0.,1.));
#16204=DIRECTION('',(0.,0.,-1.));
#16205=DIRECTION('',(0.,0.,1.));
#16206=DIRECTION('',(0.,1.,0.));
#16207=DIRECTION('center_axis',(-0.342020143325668,0.,0.939692620785909));
#16208=DIRECTION('ref_axis',(0.939692620785909,0.,0.342020143325668));
#16209=DIRECTION('',(-0.939692620785909,0.,-0.342020143325668));
#16210=DIRECTION('',(0.939692620785909,0.,0.342020143325668));
#16211=DIRECTION('',(0.,1.,0.));
#16212=DIRECTION('center_axis',(-1.,0.,0.));
#16213=DIRECTION('ref_axis',(0.,0.,1.));
#16214=DIRECTION('',(0.,0.,-1.));
#16215=DIRECTION('',(0.,0.,1.));
#16216=DIRECTION('',(0.,1.,0.));
#16217=DIRECTION('center_axis',(-0.342020143325662,0.,-0.939692620785911));
#16218=DIRECTION('ref_axis',(-0.939692620785911,0.,0.342020143325662));
#16219=DIRECTION('',(0.939692620785911,0.,-0.342020143325662));
#16220=DIRECTION('',(-0.939692620785911,0.,0.342020143325662));
#16221=DIRECTION('',(0.,1.,0.));
#16222=DIRECTION('center_axis',(-1.,0.,0.));
#16223=DIRECTION('ref_axis',(0.,0.,1.));
#16224=DIRECTION('',(0.,0.,-1.));
#16225=DIRECTION('',(0.,0.,1.));
#16226=DIRECTION('',(0.,1.,0.));
#16227=DIRECTION('center_axis',(-0.342020143325668,0.,0.939692620785909));
#16228=DIRECTION('ref_axis',(0.939692620785909,0.,0.342020143325668));
#16229=DIRECTION('',(-0.939692620785909,0.,-0.342020143325668));
#16230=DIRECTION('',(0.939692620785909,0.,0.342020143325668));
#16231=DIRECTION('',(0.,1.,0.));
#16232=DIRECTION('center_axis',(-1.,0.,0.));
#16233=DIRECTION('ref_axis',(0.,0.,1.));
#16234=DIRECTION('',(0.,0.,-1.));
#16235=DIRECTION('',(0.,0.,1.));
#16236=DIRECTION('',(0.,1.,0.));
#16237=DIRECTION('center_axis',(-0.342020143325668,0.,-0.939692620785909));
#16238=DIRECTION('ref_axis',(-0.939692620785909,0.,0.342020143325668));
#16239=DIRECTION('',(0.939692620785909,0.,-0.342020143325668));
#16240=DIRECTION('',(-0.939692620785909,0.,0.342020143325668));
#16241=DIRECTION('',(0.,1.,0.));
#16242=DIRECTION('center_axis',(-1.,0.,0.));
#16243=DIRECTION('ref_axis',(0.,0.,1.));
#16244=DIRECTION('',(0.,0.,-1.));
#16245=DIRECTION('',(0.,0.,1.));
#16246=DIRECTION('',(0.,1.,0.));
#16247=DIRECTION('center_axis',(-0.342020143325662,0.,0.939692620785911));
#16248=DIRECTION('ref_axis',(0.939692620785911,0.,0.342020143325662));
#16249=DIRECTION('',(-0.939692620785911,0.,-0.342020143325662));
#16250=DIRECTION('',(0.939692620785911,0.,0.342020143325662));
#16251=DIRECTION('',(0.,1.,0.));
#16252=DIRECTION('center_axis',(-1.,0.,0.));
#16253=DIRECTION('ref_axis',(0.,0.,1.));
#16254=DIRECTION('',(0.,0.,-1.));
#16255=DIRECTION('',(0.,0.,1.));
#16256=DIRECTION('',(0.,1.,0.));
#16257=DIRECTION('center_axis',(-0.342020143325668,0.,-0.939692620785909));
#16258=DIRECTION('ref_axis',(-0.939692620785909,0.,0.342020143325668));
#16259=DIRECTION('',(0.939692620785909,0.,-0.342020143325668));
#16260=DIRECTION('',(-0.939692620785909,0.,0.342020143325668));
#16261=DIRECTION('',(0.,1.,0.));
#16262=DIRECTION('center_axis',(-1.,0.,0.));
#16263=DIRECTION('ref_axis',(0.,0.,1.));
#16264=DIRECTION('',(0.,0.,-1.));
#16265=DIRECTION('',(0.,0.,1.));
#16266=DIRECTION('',(0.,1.,0.));
#16267=DIRECTION('center_axis',(-0.342020143325668,0.,0.939692620785909));
#16268=DIRECTION('ref_axis',(0.939692620785909,0.,0.342020143325668));
#16269=DIRECTION('',(-0.939692620785909,0.,-0.342020143325668));
#16270=DIRECTION('',(0.939692620785909,0.,0.342020143325668));
#16271=DIRECTION('',(0.,1.,0.));
#16272=DIRECTION('center_axis',(-1.,0.,0.));
#16273=DIRECTION('ref_axis',(0.,0.,1.));
#16274=DIRECTION('',(0.,0.,-1.));
#16275=DIRECTION('',(0.,0.,1.));
#16276=DIRECTION('',(0.,1.,0.));
#16277=DIRECTION('center_axis',(-0.342020143325668,0.,-0.939692620785909));
#16278=DIRECTION('ref_axis',(-0.939692620785909,0.,0.342020143325668));
#16279=DIRECTION('',(0.939692620785909,0.,-0.342020143325668));
#16280=DIRECTION('',(-0.939692620785909,0.,0.342020143325668));
#16281=DIRECTION('',(0.,1.,0.));
#16282=DIRECTION('center_axis',(-1.,0.,0.));
#16283=DIRECTION('ref_axis',(0.,0.,1.));
#16284=DIRECTION('',(0.,0.,-1.));
#16285=DIRECTION('',(0.,0.,1.));
#16286=DIRECTION('',(0.,1.,0.));
#16287=DIRECTION('center_axis',(-0.342020143325668,0.,0.939692620785909));
#16288=DIRECTION('ref_axis',(0.939692620785909,0.,0.342020143325668));
#16289=DIRECTION('',(-0.939692620785909,0.,-0.342020143325668));
#16290=DIRECTION('',(0.939692620785909,0.,0.342020143325668));
#16291=DIRECTION('',(0.,1.,0.));
#16292=DIRECTION('center_axis',(-1.,0.,0.));
#16293=DIRECTION('ref_axis',(0.,0.,1.));
#16294=DIRECTION('',(0.,0.,-1.));
#16295=DIRECTION('',(0.,0.,1.));
#16296=DIRECTION('',(0.,1.,0.));
#16297=DIRECTION('center_axis',(-0.342020143325662,0.,-0.939692620785911));
#16298=DIRECTION('ref_axis',(-0.939692620785911,0.,0.342020143325662));
#16299=DIRECTION('',(0.939692620785911,0.,-0.342020143325662));
#16300=DIRECTION('',(-0.939692620785911,0.,0.342020143325662));
#16301=DIRECTION('',(0.,1.,0.));
#16302=DIRECTION('center_axis',(-1.,0.,0.));
#16303=DIRECTION('ref_axis',(0.,0.,1.));
#16304=DIRECTION('',(0.,0.,-1.));
#16305=DIRECTION('',(0.,0.,1.));
#16306=DIRECTION('',(0.,1.,0.));
#16307=DIRECTION('center_axis',(-0.342020143325668,0.,0.939692620785909));
#16308=DIRECTION('ref_axis',(0.939692620785909,0.,0.342020143325668));
#16309=DIRECTION('',(-0.939692620785909,0.,-0.342020143325668));
#16310=DIRECTION('',(0.939692620785909,0.,0.342020143325668));
#16311=DIRECTION('',(0.,1.,0.));
#16312=DIRECTION('center_axis',(-1.,0.,0.));
#16313=DIRECTION('ref_axis',(0.,0.,1.));
#16314=DIRECTION('',(0.,0.,-1.));
#16315=DIRECTION('',(0.,0.,1.));
#16316=DIRECTION('',(0.,1.,0.));
#16317=DIRECTION('center_axis',(-0.342020143325668,0.,-0.939692620785909));
#16318=DIRECTION('ref_axis',(-0.939692620785909,0.,0.342020143325668));
#16319=DIRECTION('',(0.939692620785909,0.,-0.342020143325668));
#16320=DIRECTION('',(-0.939692620785909,0.,0.342020143325668));
#16321=DIRECTION('',(0.,1.,0.));
#16322=DIRECTION('center_axis',(-1.,0.,0.));
#16323=DIRECTION('ref_axis',(0.,0.,1.));
#16324=DIRECTION('',(0.,0.,-1.));
#16325=DIRECTION('',(0.,0.,1.));
#16326=DIRECTION('',(0.,1.,0.));
#16327=DIRECTION('center_axis',(-0.342020143325668,0.,0.939692620785909));
#16328=DIRECTION('ref_axis',(0.939692620785909,0.,0.342020143325668));
#16329=DIRECTION('',(-0.939692620785909,0.,-0.342020143325668));
#16330=DIRECTION('',(0.939692620785909,0.,0.342020143325668));
#16331=DIRECTION('',(0.,1.,0.));
#16332=DIRECTION('center_axis',(-1.,0.,0.));
#16333=DIRECTION('ref_axis',(0.,0.,1.));
#16334=DIRECTION('',(0.,0.,-1.));
#16335=DIRECTION('',(0.,0.,1.));
#16336=DIRECTION('',(0.,1.,0.));
#16337=DIRECTION('center_axis',(-0.342020143325668,0.,-0.939692620785909));
#16338=DIRECTION('ref_axis',(-0.939692620785909,0.,0.342020143325668));
#16339=DIRECTION('',(0.939692620785909,0.,-0.342020143325668));
#16340=DIRECTION('',(-0.939692620785909,0.,0.342020143325668));
#16341=DIRECTION('',(0.,1.,0.));
#16342=DIRECTION('center_axis',(-1.,0.,0.));
#16343=DIRECTION('ref_axis',(0.,0.,1.));
#16344=DIRECTION('',(0.,0.,-1.));
#16345=DIRECTION('',(0.,0.,1.));
#16346=DIRECTION('',(0.,1.,0.));
#16347=DIRECTION('center_axis',(-0.342020143325668,0.,0.939692620785909));
#16348=DIRECTION('ref_axis',(0.939692620785909,0.,0.342020143325668));
#16349=DIRECTION('',(-0.939692620785909,0.,-0.342020143325668));
#16350=DIRECTION('',(0.939692620785909,0.,0.342020143325668));
#16351=DIRECTION('',(0.,1.,0.));
#16352=DIRECTION('center_axis',(-1.,0.,0.));
#16353=DIRECTION('ref_axis',(0.,0.,1.));
#16354=DIRECTION('',(0.,0.,-1.));
#16355=DIRECTION('',(0.,0.,1.));
#16356=DIRECTION('',(0.,1.,0.));
#16357=DIRECTION('center_axis',(-0.342020143325665,0.,-0.93969262078591));
#16358=DIRECTION('ref_axis',(-0.93969262078591,0.,0.342020143325665));
#16359=DIRECTION('',(0.93969262078591,0.,-0.342020143325665));
#16360=DIRECTION('',(-0.93969262078591,0.,0.342020143325665));
#16361=DIRECTION('',(0.,1.,0.));
#16362=DIRECTION('center_axis',(-1.,0.,0.));
#16363=DIRECTION('ref_axis',(0.,0.,1.));
#16364=DIRECTION('',(0.,0.,-1.));
#16365=DIRECTION('',(0.,0.,1.));
#16366=DIRECTION('',(0.,1.,0.));
#16367=DIRECTION('center_axis',(-0.342020143325668,0.,0.939692620785909));
#16368=DIRECTION('ref_axis',(0.939692620785909,0.,0.342020143325668));
#16369=DIRECTION('',(-0.939692620785909,0.,-0.342020143325668));
#16370=DIRECTION('',(0.939692620785909,0.,0.342020143325668));
#16371=DIRECTION('',(0.,1.,0.));
#16372=DIRECTION('center_axis',(-1.,0.,0.));
#16373=DIRECTION('ref_axis',(0.,0.,1.));
#16374=DIRECTION('',(0.,0.,-1.));
#16375=DIRECTION('',(0.,0.,1.));
#16376=DIRECTION('',(0.,1.,0.));
#16377=DIRECTION('center_axis',(-0.342020143325668,0.,-0.939692620785909));
#16378=DIRECTION('ref_axis',(-0.939692620785909,0.,0.342020143325668));
#16379=DIRECTION('',(0.939692620785909,0.,-0.342020143325668));
#16380=DIRECTION('',(-0.939692620785909,0.,0.342020143325668));
#16381=DIRECTION('',(0.,1.,0.));
#16382=DIRECTION('center_axis',(-1.,0.,0.));
#16383=DIRECTION('ref_axis',(0.,0.,1.));
#16384=DIRECTION('',(0.,0.,-1.));
#16385=DIRECTION('',(0.,0.,1.));
#16386=DIRECTION('',(0.,1.,0.));
#16387=DIRECTION('center_axis',(-0.342020143325665,0.,0.93969262078591));
#16388=DIRECTION('ref_axis',(0.93969262078591,0.,0.342020143325665));
#16389=DIRECTION('',(-0.93969262078591,0.,-0.342020143325665));
#16390=DIRECTION('',(0.93969262078591,0.,0.342020143325665));
#16391=DIRECTION('',(0.,1.,0.));
#16392=DIRECTION('center_axis',(-1.,0.,0.));
#16393=DIRECTION('ref_axis',(0.,0.,1.));
#16394=DIRECTION('',(0.,0.,-1.));
#16395=DIRECTION('',(0.,0.,1.));
#16396=DIRECTION('',(0.,1.,0.));
#16397=DIRECTION('center_axis',(-0.342020143325665,0.,-0.93969262078591));
#16398=DIRECTION('ref_axis',(-0.93969262078591,0.,0.342020143325665));
#16399=DIRECTION('',(0.93969262078591,0.,-0.342020143325665));
#16400=DIRECTION('',(-0.93969262078591,0.,0.342020143325665));
#16401=DIRECTION('',(0.,1.,0.));
#16402=DIRECTION('center_axis',(-1.,0.,0.));
#16403=DIRECTION('ref_axis',(0.,0.,1.));
#16404=DIRECTION('',(0.,0.,-1.));
#16405=DIRECTION('',(0.,0.,1.));
#16406=DIRECTION('',(0.,1.,0.));
#16407=DIRECTION('center_axis',(-0.342020143325668,0.,0.939692620785909));
#16408=DIRECTION('ref_axis',(0.939692620785909,0.,0.342020143325668));
#16409=DIRECTION('',(-0.939692620785909,0.,-0.342020143325668));
#16410=DIRECTION('',(0.939692620785909,0.,0.342020143325668));
#16411=DIRECTION('',(0.,1.,0.));
#16412=DIRECTION('center_axis',(-1.,0.,0.));
#16413=DIRECTION('ref_axis',(0.,0.,1.));
#16414=DIRECTION('',(0.,0.,-1.));
#16415=DIRECTION('',(0.,0.,1.));
#16416=DIRECTION('',(0.,1.,0.));
#16417=DIRECTION('center_axis',(-0.342020143325668,0.,-0.939692620785909));
#16418=DIRECTION('ref_axis',(-0.939692620785909,0.,0.342020143325668));
#16419=DIRECTION('',(0.939692620785909,0.,-0.342020143325668));
#16420=DIRECTION('',(-0.939692620785909,0.,0.342020143325668));
#16421=DIRECTION('',(0.,1.,0.));
#16422=DIRECTION('center_axis',(-1.,0.,0.));
#16423=DIRECTION('ref_axis',(0.,0.,1.));
#16424=DIRECTION('',(0.,0.,-1.));
#16425=DIRECTION('',(0.,0.,1.));
#16426=DIRECTION('',(0.,1.,0.));
#16427=DIRECTION('center_axis',(-0.342020143325668,0.,0.939692620785909));
#16428=DIRECTION('ref_axis',(0.939692620785909,0.,0.342020143325668));
#16429=DIRECTION('',(-0.939692620785909,0.,-0.342020143325668));
#16430=DIRECTION('',(0.939692620785909,0.,0.342020143325668));
#16431=DIRECTION('',(0.,1.,0.));
#16432=DIRECTION('center_axis',(-1.,0.,0.));
#16433=DIRECTION('ref_axis',(0.,0.,1.));
#16434=DIRECTION('',(0.,0.,-1.));
#16435=DIRECTION('',(0.,0.,1.));
#16436=DIRECTION('',(0.,1.,0.));
#16437=DIRECTION('center_axis',(-0.342020143325665,0.,-0.93969262078591));
#16438=DIRECTION('ref_axis',(-0.93969262078591,0.,0.342020143325665));
#16439=DIRECTION('',(0.93969262078591,0.,-0.342020143325665));
#16440=DIRECTION('',(-0.93969262078591,0.,0.342020143325665));
#16441=DIRECTION('',(0.,1.,0.));
#16442=DIRECTION('center_axis',(-1.,0.,0.));
#16443=DIRECTION('ref_axis',(0.,0.,1.));
#16444=DIRECTION('',(0.,0.,-1.));
#16445=DIRECTION('',(0.,0.,1.));
#16446=DIRECTION('',(0.,1.,0.));
#16447=DIRECTION('center_axis',(-0.342020143325668,0.,0.939692620785909));
#16448=DIRECTION('ref_axis',(0.939692620785909,0.,0.342020143325668));
#16449=DIRECTION('',(-0.939692620785909,0.,-0.342020143325668));
#16450=DIRECTION('',(0.939692620785909,0.,0.342020143325668));
#16451=DIRECTION('',(0.,1.,0.));
#16452=DIRECTION('center_axis',(-1.,0.,0.));
#16453=DIRECTION('ref_axis',(0.,0.,1.));
#16454=DIRECTION('',(0.,0.,-1.));
#16455=DIRECTION('',(0.,0.,1.));
#16456=DIRECTION('',(0.,1.,0.));
#16457=DIRECTION('center_axis',(-0.342020143325671,0.,-0.939692620785907));
#16458=DIRECTION('ref_axis',(-0.939692620785907,0.,0.342020143325671));
#16459=DIRECTION('',(0.939692620785907,0.,-0.342020143325671));
#16460=DIRECTION('',(-0.939692620785907,0.,0.342020143325671));
#16461=DIRECTION('',(0.,1.,0.));
#16462=DIRECTION('center_axis',(-1.,0.,0.));
#16463=DIRECTION('ref_axis',(0.,0.,1.));
#16464=DIRECTION('',(0.,0.,-1.));
#16465=DIRECTION('',(0.,0.,1.));
#16466=DIRECTION('',(0.,1.,0.));
#16467=DIRECTION('center_axis',(-0.342020143325668,0.,0.939692620785909));
#16468=DIRECTION('ref_axis',(0.939692620785909,0.,0.342020143325668));
#16469=DIRECTION('',(-0.939692620785909,0.,-0.342020143325668));
#16470=DIRECTION('',(0.939692620785909,0.,0.342020143325668));
#16471=DIRECTION('',(0.,1.,0.));
#16472=DIRECTION('center_axis',(-1.,0.,0.));
#16473=DIRECTION('ref_axis',(0.,0.,1.));
#16474=DIRECTION('',(0.,0.,-1.));
#16475=DIRECTION('',(0.,0.,1.));
#16476=DIRECTION('',(0.,1.,0.));
#16477=DIRECTION('center_axis',(-0.342020143325668,0.,-0.939692620785909));
#16478=DIRECTION('ref_axis',(-0.939692620785909,0.,0.342020143325668));
#16479=DIRECTION('',(0.939692620785909,0.,-0.342020143325668));
#16480=DIRECTION('',(-0.939692620785909,0.,0.342020143325668));
#16481=DIRECTION('',(0.,1.,0.));
#16482=DIRECTION('center_axis',(-1.,0.,0.));
#16483=DIRECTION('ref_axis',(0.,0.,1.));
#16484=DIRECTION('',(0.,0.,-1.));
#16485=DIRECTION('',(0.,0.,1.));
#16486=DIRECTION('',(0.,1.,0.));
#16487=DIRECTION('center_axis',(-0.342020143325668,0.,0.939692620785909));
#16488=DIRECTION('ref_axis',(0.939692620785909,0.,0.342020143325668));
#16489=DIRECTION('',(-0.939692620785909,0.,-0.342020143325668));
#16490=DIRECTION('',(0.939692620785909,0.,0.342020143325668));
#16491=DIRECTION('',(0.,1.,0.));
#16492=DIRECTION('center_axis',(-1.,0.,0.));
#16493=DIRECTION('ref_axis',(0.,0.,1.));
#16494=DIRECTION('',(0.,0.,-1.));
#16495=DIRECTION('',(0.,0.,1.));
#16496=DIRECTION('',(0.,1.,0.));
#16497=DIRECTION('center_axis',(-0.342020143325671,0.,-0.939692620785907));
#16498=DIRECTION('ref_axis',(-0.939692620785907,0.,0.342020143325671));
#16499=DIRECTION('',(0.939692620785907,0.,-0.342020143325671));
#16500=DIRECTION('',(-0.939692620785907,0.,0.342020143325671));
#16501=DIRECTION('',(0.,1.,0.));
#16502=DIRECTION('center_axis',(-1.,0.,0.));
#16503=DIRECTION('ref_axis',(0.,0.,1.));
#16504=DIRECTION('',(0.,0.,-1.));
#16505=DIRECTION('',(0.,0.,1.));
#16506=DIRECTION('center_axis',(0.,1.,0.));
#16507=DIRECTION('ref_axis',(0.,0.,1.));
#16508=DIRECTION('center_axis',(0.,1.,0.));
#16509=DIRECTION('ref_axis',(1.,0.,0.));
#16510=DIRECTION('center_axis',(0.,0.,1.));
#16511=DIRECTION('ref_axis',(1.,0.,0.));
#16512=DIRECTION('center_axis',(0.,0.,1.));
#16513=DIRECTION('ref_axis',(1.,0.,0.));
#16514=DIRECTION('',(0.,0.,-1.));
#16515=DIRECTION('',(0.,0.,-1.));
#16516=DIRECTION('center_axis',(0.,0.,1.));
#16517=DIRECTION('ref_axis',(1.,0.,0.));
#16518=DIRECTION('center_axis',(0.,0.,1.));
#16519=DIRECTION('ref_axis',(1.,0.,0.));
#16520=DIRECTION('center_axis',(0.,0.,1.));
#16521=DIRECTION('ref_axis',(1.,0.,0.));
#16522=DIRECTION('axis',(0.,0.,1.));
#16523=DIRECTION('refdir',(1.,0.,0.));
#16524=DIRECTION('center_axis',(0.,0.,1.));
#16525=DIRECTION('ref_axis',(1.,0.,0.));
#16526=DIRECTION('center_axis',(0.,0.,1.));
#16527=DIRECTION('ref_axis',(1.,0.,0.));
#16528=DIRECTION('',(0.,0.,-1.));
#16529=DIRECTION('center_axis',(0.,0.,-1.));
#16530=DIRECTION('ref_axis',(1.,0.,0.));
#16531=DIRECTION('center_axis',(0.,0.,1.));
#16532=DIRECTION('ref_axis',(1.,0.,0.));
#16533=DIRECTION('center_axis',(0.,0.,1.));
#16534=DIRECTION('ref_axis',(1.,0.,0.));
#16535=DIRECTION('center_axis',(0.,0.,1.));
#16536=DIRECTION('ref_axis',(1.,0.,0.));
#16537=DIRECTION('',(0.,0.,-1.));
#16538=DIRECTION('center_axis',(0.,0.,1.));
#16539=DIRECTION('ref_axis',(1.,0.,0.));
#16540=DIRECTION('center_axis',(0.,0.,1.));
#16541=DIRECTION('ref_axis',(1.,0.,0.));
#16542=DIRECTION('center_axis',(0.,0.,1.));
#16543=DIRECTION('ref_axis',(1.,0.,0.));
#16544=DIRECTION('axis',(0.,0.,1.));
#16545=DIRECTION('refdir',(1.,0.,0.));
#16546=DIRECTION('center_axis',(1.,0.,0.));
#16547=DIRECTION('ref_axis',(0.,0.,-1.));
#16548=DIRECTION('',(1.,0.,0.));
#16549=DIRECTION('center_axis',(0.,1.,0.));
#16550=DIRECTION('ref_axis',(-1.,0.,0.));
#16551=DIRECTION('',(-1.,0.,0.));
#16552=DIRECTION('',(0.,0.,1.));
#16553=DIRECTION('',(1.,0.,0.));
#16554=DIRECTION('',(0.,0.,1.));
#16555=DIRECTION('center_axis',(1.,0.,0.));
#16556=DIRECTION('ref_axis',(0.,1.,0.));
#16557=DIRECTION('',(0.,1.,0.));
#16558=DIRECTION('',(0.,0.,1.));
#16559=DIRECTION('',(0.,-1.,0.));
#16560=DIRECTION('',(0.,0.,1.));
#16561=DIRECTION('center_axis',(1.,0.,0.));
#16562=DIRECTION('ref_axis',(0.,1.,0.));
#16563=DIRECTION('',(0.,1.,0.));
#16564=DIRECTION('',(0.,0.,-1.));
#16565=DIRECTION('',(0.,-1.,0.));
#16566=DIRECTION('center_axis',(0.,-1.,0.));
#16567=DIRECTION('ref_axis',(1.,0.,0.));
#16568=DIRECTION('',(1.,0.,0.));
#16569=DIRECTION('',(0.,0.,-1.));
#16570=DIRECTION('',(-1.,0.,0.));
#16571=DIRECTION('center_axis',(0.,0.,1.));
#16572=DIRECTION('ref_axis',(1.,0.,0.));
#16573=DIRECTION('center_axis',(0.,0.,-1.));
#16574=DIRECTION('ref_axis',(1.,0.,0.));
#16575=DIRECTION('center_axis',(0.,0.,1.));
#16576=DIRECTION('ref_axis',(1.,0.,0.));
#16577=DIRECTION('center_axis',(0.,0.,1.));
#16578=DIRECTION('ref_axis',(1.,0.,0.));
#16579=DIRECTION('center_axis',(0.,0.,1.));
#16580=DIRECTION('ref_axis',(1.,0.,0.));
#16581=DIRECTION('center_axis',(0.,0.,1.));
#16582=DIRECTION('ref_axis',(1.,0.,0.));
#16583=DIRECTION('center_axis',(0.,0.,-1.));
#16584=DIRECTION('ref_axis',(1.,0.,0.));
#16585=DIRECTION('center_axis',(0.,0.,1.));
#16586=DIRECTION('ref_axis',(1.,0.,0.));
#16587=DIRECTION('axis',(0.,0.,1.));
#16588=DIRECTION('refdir',(1.,0.,0.));
#16589=DIRECTION('center_axis',(0.866025403784439,0.,-0.5));
#16590=DIRECTION('ref_axis',(0.5,0.,0.866025403784439));
#16591=DIRECTION('',(0.5,0.,0.866025403784439));
#16592=DIRECTION('',(0.,-1.,0.));
#16593=DIRECTION('',(0.5,0.,0.866025403784439));
#16594=DIRECTION('',(0.,-1.,0.));
#16595=DIRECTION('center_axis',(1.20185167898973E-16,0.,-1.));
#16596=DIRECTION('ref_axis',(1.,0.,1.20185167898973E-16));
#16597=DIRECTION('',(1.,0.,1.20185167898973E-16));
#16598=DIRECTION('',(0.,-1.,0.));
#16599=DIRECTION('',(1.,0.,1.20185167898973E-16));
#16600=DIRECTION('center_axis',(-0.866025403784439,0.,-0.5));
#16601=DIRECTION('ref_axis',(0.5,0.,-0.866025403784439));
#16602=DIRECTION('',(0.5,0.,-0.866025403784439));
#16603=DIRECTION('',(0.,-1.,0.));
#16604=DIRECTION('',(0.5,0.,-0.866025403784439));
#16605=DIRECTION('center_axis',(-0.866025403784439,0.,0.5));
#16606=DIRECTION('ref_axis',(-0.5,0.,-0.866025403784439));
#16607=DIRECTION('',(-0.5,0.,-0.866025403784439));
#16608=DIRECTION('',(0.,-1.,0.));
#16609=DIRECTION('',(-0.5,0.,-0.866025403784439));
#16610=DIRECTION('center_axis',(-2.40370335797945E-16,0.,1.));
#16611=DIRECTION('ref_axis',(-1.,0.,-2.40370335797945E-16));
#16612=DIRECTION('',(-1.,0.,-2.40370335797945E-16));
#16613=DIRECTION('',(0.,-1.,0.));
#16614=DIRECTION('',(-1.,0.,-2.40370335797945E-16));
#16615=DIRECTION('center_axis',(0.866025403784439,0.,0.5));
#16616=DIRECTION('ref_axis',(-0.5,0.,0.866025403784439));
#16617=DIRECTION('',(-0.5,0.,0.866025403784439));
#16618=DIRECTION('',(-0.5,0.,0.866025403784439));
#16619=DIRECTION('center_axis',(0.,-1.,0.));
#16620=DIRECTION('ref_axis',(0.,0.,-1.));
#16621=DIRECTION('center_axis',(0.,1.,0.));
#16622=DIRECTION('ref_axis',(0.,0.,1.));
#16623=DIRECTION('center_axis',(0.,-1.,0.));
#16624=DIRECTION('ref_axis',(1.,0.,0.));
#16625=DIRECTION('center_axis',(0.,-1.,0.));
#16626=DIRECTION('ref_axis',(1.,0.,0.));
#16627=DIRECTION('center_axis',(0.,-1.,0.));
#16628=DIRECTION('ref_axis',(1.,0.,0.));
#16629=DIRECTION('',(0.707106781186548,0.707106781186547,8.65956056235494E-17));
#16630=DIRECTION('center_axis',(0.,-1.,0.));
#16631=DIRECTION('ref_axis',(1.,0.,0.));
#16632=DIRECTION('center_axis',(0.,1.,0.));
#16633=DIRECTION('ref_axis',(1.,0.,0.));
#16634=DIRECTION('',(0.,1.,0.));
#16635=DIRECTION('center_axis',(0.,1.,0.));
#16636=DIRECTION('ref_axis',(1.,0.,0.));
#16637=DIRECTION('center_axis',(0.,-1.,0.));
#16638=DIRECTION('ref_axis',(1.,0.,0.));
#16639=DIRECTION('',(-0.707106781186548,0.707106781186547,-8.65956056235494E-17));
#16640=DIRECTION('center_axis',(0.,-1.,0.));
#16641=DIRECTION('ref_axis',(0.,0.,-1.));
#16642=DIRECTION('',(0.,0.,1.));
#16643=DIRECTION('',(1.,0.,0.));
#16644=DIRECTION('',(0.,0.,1.));
#16645=DIRECTION('',(1.,0.,0.));
#16646=DIRECTION('',(0.,0.,1.));
#16647=DIRECTION('',(1.,0.,0.));
#16648=DIRECTION('',(0.,0.,1.));
#16649=DIRECTION('',(2.22044604925031E-16,-1.,0.));
#16650=DIRECTION('axis',(0.,0.,1.));
#16651=DIRECTION('refdir',(1.,0.,0.));
#16652=DIRECTION('axis',(0.,0.,1.));
#16653=DIRECTION('refdir',(1.,0.,0.));
#16654=DIRECTION('center_axis',(0.,1.,0.));
#16655=DIRECTION('ref_axis',(1.,0.,0.));
#16656=DIRECTION('center_axis',(0.,1.,0.));
#16657=DIRECTION('ref_axis',(1.,0.,0.));
#16658=DIRECTION('',(0.,1.,0.));
#16659=DIRECTION('center_axis',(0.,-1.,0.));
#16660=DIRECTION('ref_axis',(1.,0.,0.));
#16661=DIRECTION('center_axis',(0.,1.,0.));
#16662=DIRECTION('ref_axis',(1.,0.,0.));
#16663=DIRECTION('center_axis',(0.,1.,0.));
#16664=DIRECTION('ref_axis',(1.,0.,0.));
#16665=DIRECTION('center_axis',(0.,1.,0.));
#16666=DIRECTION('ref_axis',(1.,0.,0.));
#16667=DIRECTION('',(0.,1.,0.));
#16668=DIRECTION('center_axis',(0.,1.,0.));
#16669=DIRECTION('ref_axis',(1.,0.,0.));
#16670=DIRECTION('center_axis',(0.,1.,0.));
#16671=DIRECTION('ref_axis',(1.,0.,0.));
#16672=DIRECTION('center_axis',(0.,0.,-1.));
#16673=DIRECTION('ref_axis',(-1.,0.,0.));
#16674=DIRECTION('',(0.,-1.,0.));
#16675=DIRECTION('',(-1.,0.,0.));
#16676=DIRECTION('',(0.,1.,0.));
#16677=DIRECTION('',(1.,0.,0.));
#16678=DIRECTION('center_axis',(0.,1.,0.));
#16679=DIRECTION('ref_axis',(1.,0.,0.));
#16680=DIRECTION('center_axis',(0.,-1.,0.));
#16681=DIRECTION('ref_axis',(1.,0.,0.));
#16682=DIRECTION('',(0.,0.,-1.));
#16683=DIRECTION('',(-1.,0.,0.));
#16684=DIRECTION('center_axis',(-1.,0.,0.));
#16685=DIRECTION('ref_axis',(0.,0.,1.));
#16686=DIRECTION('',(0.,0.,1.));
#16687=DIRECTION('',(0.,1.,0.));
#16688=DIRECTION('center_axis',(0.,0.,1.));
#16689=DIRECTION('ref_axis',(1.,0.,0.));
#16690=DIRECTION('',(0.,1.,0.));
#16691=DIRECTION('',(1.,0.,0.));
#16692=DIRECTION('center_axis',(0.,1.,0.));
#16693=DIRECTION('ref_axis',(0.,0.,1.));
#16694=DIRECTION('center_axis',(0.,1.,0.));
#16695=DIRECTION('ref_axis',(1.,0.,0.));
#16696=DIRECTION('center_axis',(0.,0.,-1.));
#16697=DIRECTION('ref_axis',(-1.,0.,0.));
#16698=DIRECTION('',(0.,-1.,0.));
#16699=DIRECTION('',(-1.,0.,0.));
#16700=DIRECTION('',(0.,1.,0.));
#16701=DIRECTION('',(1.,0.,0.));
#16702=DIRECTION('center_axis',(0.,1.,0.));
#16703=DIRECTION('ref_axis',(1.,0.,0.));
#16704=DIRECTION('center_axis',(0.,-1.,0.));
#16705=DIRECTION('ref_axis',(1.,0.,0.));
#16706=DIRECTION('',(0.,0.,-1.));
#16707=DIRECTION('',(-1.,0.,0.));
#16708=DIRECTION('center_axis',(-1.,0.,0.));
#16709=DIRECTION('ref_axis',(0.,0.,1.));
#16710=DIRECTION('',(0.,0.,1.));
#16711=DIRECTION('',(0.,1.,0.));
#16712=DIRECTION('center_axis',(0.,0.,1.));
#16713=DIRECTION('ref_axis',(1.,0.,0.));
#16714=DIRECTION('',(0.,1.,0.));
#16715=DIRECTION('',(1.,0.,0.));
#16716=DIRECTION('center_axis',(0.,1.,0.));
#16717=DIRECTION('ref_axis',(0.,0.,1.));
#16718=DIRECTION('center_axis',(0.,1.,0.));
#16719=DIRECTION('ref_axis',(1.,0.,0.));
#16720=DIRECTION('center_axis',(0.,1.,0.));
#16721=DIRECTION('ref_axis',(1.,0.,0.));
#16722=DIRECTION('center_axis',(0.,1.,0.));
#16723=DIRECTION('ref_axis',(1.,0.,0.));
#16724=DIRECTION('',(0.,-1.,0.));
#16725=DIRECTION('center_axis',(0.,1.,0.));
#16726=DIRECTION('ref_axis',(1.,0.,0.));
#16727=DIRECTION('center_axis',(0.,1.,0.));
#16728=DIRECTION('ref_axis',(1.,0.,0.));
#16729=DIRECTION('center_axis',(0.,1.,0.));
#16730=DIRECTION('ref_axis',(1.,0.,0.));
#16731=DIRECTION('axis',(0.,0.,1.));
#16732=DIRECTION('refdir',(1.,0.,0.));
#16733=DIRECTION('center_axis',(0.,1.,0.));
#16734=DIRECTION('ref_axis',(1.,0.,0.));
#16735=DIRECTION('center_axis',(0.,-1.,0.));
#16736=DIRECTION('ref_axis',(1.,0.,0.));
#16737=DIRECTION('',(0.,-1.,0.));
#16738=DIRECTION('center_axis',(0.,-1.,0.));
#16739=DIRECTION('ref_axis',(1.,0.,0.));
#16740=DIRECTION('center_axis',(0.,1.,0.));
#16741=DIRECTION('ref_axis',(1.,0.,0.));
#16742=DIRECTION('center_axis',(0.,1.,0.));
#16743=DIRECTION('ref_axis',(1.,0.,0.));
#16744=DIRECTION('',(0.,-1.,0.));
#16745=DIRECTION('center_axis',(0.,1.,0.));
#16746=DIRECTION('ref_axis',(1.,0.,0.));
#16747=DIRECTION('center_axis',(0.,1.,0.));
#16748=DIRECTION('ref_axis',(1.,0.,0.));
#16749=DIRECTION('center_axis',(0.,1.,0.));
#16750=DIRECTION('ref_axis',(1.,0.,0.));
#16751=DIRECTION('axis',(0.,0.,1.));
#16752=DIRECTION('refdir',(1.,0.,0.));
#16753=DIRECTION('center_axis',(0.,1.,0.));
#16754=DIRECTION('ref_axis',(1.,0.,0.));
#16755=DIRECTION('center_axis',(0.,-1.,0.));
#16756=DIRECTION('ref_axis',(1.,0.,0.));
#16757=DIRECTION('',(0.,-1.,0.));
#16758=DIRECTION('center_axis',(0.,-1.,0.));
#16759=DIRECTION('ref_axis',(1.,0.,0.));
#16760=DIRECTION('center_axis',(0.,1.,0.));
#16761=DIRECTION('ref_axis',(1.,0.,0.));
#16762=DIRECTION('center_axis',(0.,1.,0.));
#16763=DIRECTION('ref_axis',(1.,0.,0.));
#16764=DIRECTION('',(0.,-1.,0.));
#16765=DIRECTION('center_axis',(0.,1.,0.));
#16766=DIRECTION('ref_axis',(1.,0.,0.));
#16767=DIRECTION('center_axis',(0.,1.,0.));
#16768=DIRECTION('ref_axis',(1.,0.,0.));
#16769=DIRECTION('center_axis',(0.,1.,0.));
#16770=DIRECTION('ref_axis',(1.,0.,0.));
#16771=DIRECTION('axis',(0.,0.,1.));
#16772=DIRECTION('refdir',(1.,0.,0.));
#16773=DIRECTION('center_axis',(0.,1.,0.));
#16774=DIRECTION('ref_axis',(1.,0.,0.));
#16775=DIRECTION('center_axis',(0.,-1.,0.));
#16776=DIRECTION('ref_axis',(1.,0.,0.));
#16777=DIRECTION('',(0.,-1.,0.));
#16778=DIRECTION('center_axis',(0.,-1.,0.));
#16779=DIRECTION('ref_axis',(1.,0.,0.));
#16780=DIRECTION('center_axis',(0.,1.,0.));
#16781=DIRECTION('ref_axis',(1.,0.,0.));
#16782=DIRECTION('center_axis',(0.,1.,0.));
#16783=DIRECTION('ref_axis',(1.,0.,0.));
#16784=DIRECTION('',(0.,-1.,0.));
#16785=DIRECTION('center_axis',(0.,1.,0.));
#16786=DIRECTION('ref_axis',(1.,0.,0.));
#16787=DIRECTION('center_axis',(0.,1.,0.));
#16788=DIRECTION('ref_axis',(1.,0.,0.));
#16789=DIRECTION('center_axis',(0.,1.,0.));
#16790=DIRECTION('ref_axis',(1.,0.,0.));
#16791=DIRECTION('axis',(0.,0.,1.));
#16792=DIRECTION('refdir',(1.,0.,0.));
#16793=DIRECTION('center_axis',(0.,1.,0.));
#16794=DIRECTION('ref_axis',(1.,0.,0.));
#16795=DIRECTION('center_axis',(0.,-1.,0.));
#16796=DIRECTION('ref_axis',(1.,0.,0.));
#16797=DIRECTION('',(0.,-1.,0.));
#16798=DIRECTION('center_axis',(0.,-1.,0.));
#16799=DIRECTION('ref_axis',(1.,0.,0.));
#16800=DIRECTION('center_axis',(0.,1.,0.));
#16801=DIRECTION('ref_axis',(1.,0.,0.));
#16802=DIRECTION('center_axis',(0.,1.,0.));
#16803=DIRECTION('ref_axis',(1.,0.,0.));
#16804=DIRECTION('',(0.,-1.,0.));
#16805=DIRECTION('center_axis',(0.,1.,0.));
#16806=DIRECTION('ref_axis',(1.,0.,0.));
#16807=DIRECTION('center_axis',(0.,1.,0.));
#16808=DIRECTION('ref_axis',(1.,0.,0.));
#16809=DIRECTION('center_axis',(0.,1.,0.));
#16810=DIRECTION('ref_axis',(1.,0.,0.));
#16811=DIRECTION('axis',(0.,0.,1.));
#16812=DIRECTION('refdir',(1.,0.,0.));
#16813=DIRECTION('center_axis',(0.,1.,0.));
#16814=DIRECTION('ref_axis',(-1.,0.,0.));
#16815=DIRECTION('',(-1.,0.,0.));
#16816=DIRECTION('',(0.,0.,1.));
#16817=DIRECTION('',(-1.,0.,0.));
#16818=DIRECTION('',(0.,0.,1.));
#16819=DIRECTION('center_axis',(1.,0.,0.));
#16820=DIRECTION('ref_axis',(0.,1.,0.));
#16821=DIRECTION('',(0.,1.,0.));
#16822=DIRECTION('',(0.,1.,0.));
#16823=DIRECTION('',(0.,0.,1.));
#16824=DIRECTION('center_axis',(0.,-1.,0.));
#16825=DIRECTION('ref_axis',(1.,0.,0.));
#16826=DIRECTION('',(1.,0.,0.));
#16827=DIRECTION('',(1.,0.,0.));
#16828=DIRECTION('',(0.,0.,1.));
#16829=DIRECTION('center_axis',(-1.,0.,0.));
#16830=DIRECTION('ref_axis',(0.,-1.,0.));
#16831=DIRECTION('',(0.,-1.,0.));
#16832=DIRECTION('',(0.,-1.,0.));
#16833=DIRECTION('center_axis',(0.,0.,1.));
#16834=DIRECTION('ref_axis',(1.,0.,0.));
#16835=DIRECTION('center_axis',(0.,0.,1.));
#16836=DIRECTION('ref_axis',(1.,0.,0.));
#16837=DIRECTION('axis',(0.,0.,1.));
#16838=DIRECTION('refdir',(1.,0.,0.));
#16839=DIRECTION('center_axis',(0.,1.,0.));
#16840=DIRECTION('ref_axis',(-1.,0.,0.));
#16841=DIRECTION('',(-1.,0.,0.));
#16842=DIRECTION('',(0.,0.,1.));
#16843=DIRECTION('',(-1.,0.,0.));
#16844=DIRECTION('',(0.,0.,1.));
#16845=DIRECTION('center_axis',(1.,0.,0.));
#16846=DIRECTION('ref_axis',(0.,1.,0.));
#16847=DIRECTION('',(0.,1.,0.));
#16848=DIRECTION('',(0.,1.,0.));
#16849=DIRECTION('',(0.,0.,1.));
#16850=DIRECTION('center_axis',(0.,-1.,0.));
#16851=DIRECTION('ref_axis',(1.,0.,0.));
#16852=DIRECTION('',(1.,0.,0.));
#16853=DIRECTION('',(1.,0.,0.));
#16854=DIRECTION('',(0.,0.,1.));
#16855=DIRECTION('center_axis',(-1.,0.,0.));
#16856=DIRECTION('ref_axis',(0.,-1.,0.));
#16857=DIRECTION('',(0.,-1.,0.));
#16858=DIRECTION('',(0.,-1.,0.));
#16859=DIRECTION('center_axis',(0.,0.,1.));
#16860=DIRECTION('ref_axis',(1.,0.,0.));
#16861=DIRECTION('center_axis',(0.,0.,1.));
#16862=DIRECTION('ref_axis',(1.,0.,0.));
#16863=DIRECTION('axis',(0.,0.,1.));
#16864=DIRECTION('refdir',(1.,0.,0.));
#16865=DIRECTION('center_axis',(0.,1.,0.));
#16866=DIRECTION('ref_axis',(1.,0.,0.));
#16867=DIRECTION('center_axis',(0.,1.,0.));
#16868=DIRECTION('ref_axis',(1.,0.,0.));
#16869=DIRECTION('',(0.,1.,0.));
#16870=DIRECTION('center_axis',(0.,-1.,0.));
#16871=DIRECTION('ref_axis',(1.,0.,0.));
#16872=DIRECTION('center_axis',(0.,0.,-1.));
#16873=DIRECTION('ref_axis',(-1.,0.,0.));
#16874=DIRECTION('',(-1.,0.,0.));
#16875=DIRECTION('',(0.,1.,0.));
#16876=DIRECTION('',(1.,0.,0.));
#16877=DIRECTION('',(0.,1.,0.));
#16878=DIRECTION('center_axis',(1.,0.,0.));
#16879=DIRECTION('ref_axis',(0.,0.,-1.));
#16880=DIRECTION('',(0.,0.,-1.));
#16881=DIRECTION('',(0.,1.,0.));
#16882=DIRECTION('',(0.,0.,1.));
#16883=DIRECTION('center_axis',(0.,0.,1.));
#16884=DIRECTION('ref_axis',(1.,0.,0.));
#16885=DIRECTION('',(1.,0.,0.));
#16886=DIRECTION('',(0.,-1.,0.));
#16887=DIRECTION('',(-1.,0.,0.));
#16888=DIRECTION('center_axis',(0.,1.,0.));
#16889=DIRECTION('ref_axis',(1.,0.,0.));
#16890=DIRECTION('center_axis',(0.,1.,0.));
#16891=DIRECTION('ref_axis',(1.,0.,0.));
#16892=DIRECTION('center_axis',(0.,-1.,0.));
#16893=DIRECTION('ref_axis',(1.,0.,0.));
#16894=DIRECTION('center_axis',(0.,1.,0.));
#16895=DIRECTION('ref_axis',(-1.,0.,-1.22464679914735E-16));
#16896=DIRECTION('center_axis',(0.,-1.,0.));
#16897=DIRECTION('ref_axis',(1.,0.,0.));
#16898=DIRECTION('center_axis',(0.,1.,0.));
#16899=DIRECTION('ref_axis',(6.12323399573677E-17,0.,1.));
#16900=DIRECTION('',(0.,-1.,0.));
#16901=DIRECTION('center_axis',(0.,1.,0.));
#16902=DIRECTION('ref_axis',(1.,0.,0.));
#16903=DIRECTION('',(0.,1.,0.));
#16904=DIRECTION('center_axis',(0.,1.,0.));
#16905=DIRECTION('ref_axis',(1.,0.,0.));
#16906=DIRECTION('center_axis',(1.,0.,0.));
#16907=DIRECTION('ref_axis',(0.,0.,-1.));
#16908=DIRECTION('',(0.,0.,1.));
#16909=DIRECTION('',(0.,-1.,0.));
#16910=DIRECTION('',(0.,0.,-1.));
#16911=DIRECTION('center_axis',(0.,1.,0.));
#16912=DIRECTION('ref_axis',(1.,0.,0.));
#16913=DIRECTION('',(0.,0.,-1.));
#16914=DIRECTION('center_axis',(0.,-1.,0.));
#16915=DIRECTION('ref_axis',(1.,0.,0.));
#16916=DIRECTION('center_axis',(-1.,0.,0.));
#16917=DIRECTION('ref_axis',(0.,0.,1.));
#16918=DIRECTION('',(0.,0.,1.));
#16919=DIRECTION('',(0.,1.,0.));
#16920=DIRECTION('center_axis',(0.,1.,0.));
#16921=DIRECTION('ref_axis',(0.,0.,1.));
#16922=DIRECTION('center_axis',(0.,1.,0.));
#16923=DIRECTION('ref_axis',(1.,0.,0.));
#16924=DIRECTION('center_axis',(0.,1.,0.));
#16925=DIRECTION('ref_axis',(1.,0.,0.));
#16926=DIRECTION('',(0.,-1.,0.));
#16927=DIRECTION('center_axis',(0.,1.,0.));
#16928=DIRECTION('ref_axis',(1.,0.,0.));
#16929=DIRECTION('center_axis',(0.,1.,0.));
#16930=DIRECTION('ref_axis',(1.,0.,0.));
#16931=DIRECTION('axis',(0.,0.,1.));
#16932=DIRECTION('refdir',(1.,0.,0.));
#16933=DIRECTION('center_axis',(0.,1.,0.));
#16934=DIRECTION('ref_axis',(1.,0.,0.));
#16935=DIRECTION('center_axis',(0.,-1.,0.));
#16936=DIRECTION('ref_axis',(1.,0.,0.));
#16937=DIRECTION('',(0.,-1.,0.));
#16938=DIRECTION('center_axis',(0.,-1.,0.));
#16939=DIRECTION('ref_axis',(1.,0.,0.));
#16940=DIRECTION('center_axis',(0.,1.,0.));
#16941=DIRECTION('ref_axis',(1.,0.,0.));
#16942=DIRECTION('center_axis',(0.,1.,0.));
#16943=DIRECTION('ref_axis',(1.,0.,0.));
#16944=DIRECTION('',(0.,-1.,0.));
#16945=DIRECTION('center_axis',(0.,1.,0.));
#16946=DIRECTION('ref_axis',(1.,0.,0.));
#16947=DIRECTION('center_axis',(0.,1.,0.));
#16948=DIRECTION('ref_axis',(1.,0.,0.));
#16949=DIRECTION('center_axis',(0.,1.,0.));
#16950=DIRECTION('ref_axis',(1.,0.,0.));
#16951=DIRECTION('axis',(0.,0.,1.));
#16952=DIRECTION('refdir',(1.,0.,0.));
#16953=DIRECTION('center_axis',(0.,1.,0.));
#16954=DIRECTION('ref_axis',(1.,0.,0.));
#16955=DIRECTION('center_axis',(0.,-1.,0.));
#16956=DIRECTION('ref_axis',(1.,0.,0.));
#16957=DIRECTION('',(0.,-1.,0.));
#16958=DIRECTION('center_axis',(0.,-1.,0.));
#16959=DIRECTION('ref_axis',(1.,0.,0.));
#16960=DIRECTION('center_axis',(0.,1.,0.));
#16961=DIRECTION('ref_axis',(1.,0.,0.));
#16962=DIRECTION('center_axis',(0.,1.,0.));
#16963=DIRECTION('ref_axis',(1.,0.,0.));
#16964=DIRECTION('',(0.,-1.,0.));
#16965=DIRECTION('center_axis',(0.,1.,0.));
#16966=DIRECTION('ref_axis',(1.,0.,0.));
#16967=DIRECTION('center_axis',(0.,1.,0.));
#16968=DIRECTION('ref_axis',(1.,0.,0.));
#16969=DIRECTION('center_axis',(0.,1.,0.));
#16970=DIRECTION('ref_axis',(1.,0.,0.));
#16971=DIRECTION('axis',(0.,0.,1.));
#16972=DIRECTION('refdir',(1.,0.,0.));
#16973=DIRECTION('center_axis',(0.,1.,0.));
#16974=DIRECTION('ref_axis',(1.,0.,0.));
#16975=DIRECTION('center_axis',(0.,-1.,0.));
#16976=DIRECTION('ref_axis',(1.,0.,0.));
#16977=DIRECTION('',(0.,-1.,0.));
#16978=DIRECTION('center_axis',(0.,-1.,0.));
#16979=DIRECTION('ref_axis',(1.,0.,0.));
#16980=DIRECTION('center_axis',(0.,1.,0.));
#16981=DIRECTION('ref_axis',(1.,0.,0.));
#16982=DIRECTION('center_axis',(0.,1.,0.));
#16983=DIRECTION('ref_axis',(1.,0.,0.));
#16984=DIRECTION('',(0.,-1.,0.));
#16985=DIRECTION('center_axis',(0.,1.,0.));
#16986=DIRECTION('ref_axis',(1.,0.,0.));
#16987=DIRECTION('center_axis',(0.,1.,0.));
#16988=DIRECTION('ref_axis',(1.,0.,0.));
#16989=DIRECTION('center_axis',(0.,1.,0.));
#16990=DIRECTION('ref_axis',(1.,0.,0.));
#16991=DIRECTION('axis',(0.,0.,1.));
#16992=DIRECTION('refdir',(1.,0.,0.));
#16993=DIRECTION('center_axis',(1.,0.,0.));
#16994=DIRECTION('ref_axis',(0.,0.,-1.));
#16995=DIRECTION('',(0.,0.,1.));
#16996=DIRECTION('',(0.,1.,0.));
#16997=DIRECTION('',(0.,0.,-1.));
#16998=DIRECTION('',(0.,-1.,0.));
#16999=DIRECTION('center_axis',(0.,0.,-1.));
#17000=DIRECTION('ref_axis',(-1.,0.,0.));
#17001=DIRECTION('',(1.,0.,0.));
#17002=DIRECTION('',(0.,-1.,0.));
#17003=DIRECTION('',(-1.,0.,0.));
#17004=DIRECTION('center_axis',(-1.,0.,0.));
#17005=DIRECTION('ref_axis',(0.,0.,1.));
#17006=DIRECTION('',(0.,0.,-1.));
#17007=DIRECTION('',(0.,1.,0.));
#17008=DIRECTION('',(0.,0.,1.));
#17009=DIRECTION('center_axis',(0.,1.,0.));
#17010=DIRECTION('ref_axis',(1.,0.,0.));
#17011=DIRECTION('center_axis',(0.,-1.,0.));
#17012=DIRECTION('ref_axis',(1.,0.,0.));
#17013=DIRECTION('',(-0.587785252292473,0.,0.809016994374947));
#17014=DIRECTION('center_axis',(0.,-1.,0.));
#17015=DIRECTION('ref_axis',(1.,0.,0.));
#17016=DIRECTION('',(-0.809016994374948,0.,0.587785252292473));
#17017=DIRECTION('center_axis',(0.,-1.,0.));
#17018=DIRECTION('ref_axis',(1.,0.,0.));
#17019=DIRECTION('',(-0.951056516295154,0.,0.309016994374947));
#17020=DIRECTION('center_axis',(0.,-1.,0.));
#17021=DIRECTION('ref_axis',(1.,0.,0.));
#17022=DIRECTION('',(-1.,0.,-1.83697019872103E-16));
#17023=DIRECTION('center_axis',(0.,-1.,0.));
#17024=DIRECTION('ref_axis',(1.,0.,0.));
#17025=DIRECTION('',(-0.951056516295154,0.,-0.309016994374948));
#17026=DIRECTION('center_axis',(0.,-1.,0.));
#17027=DIRECTION('ref_axis',(1.,0.,0.));
#17028=DIRECTION('',(-0.809016994374947,0.,-0.587785252292473));
#17029=DIRECTION('center_axis',(0.,-1.,0.));
#17030=DIRECTION('ref_axis',(1.,0.,0.));
#17031=DIRECTION('',(-0.587785252292473,0.,-0.809016994374948));
#17032=DIRECTION('center_axis',(0.,-1.,0.));
#17033=DIRECTION('ref_axis',(1.,0.,0.));
#17034=DIRECTION('',(-0.309016994374947,0.,-0.951056516295154));
#17035=DIRECTION('center_axis',(0.,-1.,0.));
#17036=DIRECTION('ref_axis',(1.,0.,0.));
#17037=DIRECTION('',(1.22464679914735E-16,0.,-1.));
#17038=DIRECTION('center_axis',(0.,-1.,0.));
#17039=DIRECTION('ref_axis',(1.,0.,0.));
#17040=DIRECTION('',(0.309016994374948,0.,-0.951056516295154));
#17041=DIRECTION('center_axis',(0.,-1.,0.));
#17042=DIRECTION('ref_axis',(1.,0.,0.));
#17043=DIRECTION('',(0.587785252292473,0.,-0.809016994374947));
#17044=DIRECTION('center_axis',(0.,-1.,0.));
#17045=DIRECTION('ref_axis',(1.,0.,0.));
#17046=DIRECTION('',(0.809016994374948,0.,-0.587785252292473));
#17047=DIRECTION('center_axis',(0.,-1.,0.));
#17048=DIRECTION('ref_axis',(1.,0.,0.));
#17049=DIRECTION('',(0.951056516295154,0.,-0.309016994374947));
#17050=DIRECTION('center_axis',(0.,-1.,0.));
#17051=DIRECTION('ref_axis',(1.,0.,0.));
#17052=DIRECTION('',(1.,0.,6.12323399573677E-17));
#17053=DIRECTION('center_axis',(0.,-1.,0.));
#17054=DIRECTION('ref_axis',(1.,0.,0.));
#17055=DIRECTION('',(0.951056516295154,0.,0.309016994374948));
#17056=DIRECTION('center_axis',(0.,-1.,0.));
#17057=DIRECTION('ref_axis',(1.,0.,0.));
#17058=DIRECTION('',(0.809016994374947,0.,0.587785252292473));
#17059=DIRECTION('center_axis',(0.,-1.,0.));
#17060=DIRECTION('ref_axis',(1.,0.,0.));
#17061=DIRECTION('',(0.587785252292473,0.,0.809016994374947));
#17062=DIRECTION('center_axis',(0.,-1.,0.));
#17063=DIRECTION('ref_axis',(1.,0.,0.));
#17064=DIRECTION('',(0.309016994374947,0.,0.951056516295154));
#17065=DIRECTION('center_axis',(0.,-1.,0.));
#17066=DIRECTION('ref_axis',(1.,0.,0.));
#17067=DIRECTION('',(0.,0.,1.));
#17068=DIRECTION('center_axis',(0.,-1.,0.));
#17069=DIRECTION('ref_axis',(1.,0.,0.));
#17070=DIRECTION('',(-0.309016994374948,0.,0.951056516295154));
#17071=DIRECTION('center_axis',(0.,1.,0.));
#17072=DIRECTION('ref_axis',(1.,0.,0.));
#17073=DIRECTION('center_axis',(0.,1.,0.));
#17074=DIRECTION('ref_axis',(6.12323399573677E-17,0.,1.));
#17075=DIRECTION('center_axis',(0.,-1.,0.));
#17076=DIRECTION('ref_axis',(1.,0.,0.));
#17077=DIRECTION('center_axis',(0.,1.,0.));
#17078=DIRECTION('ref_axis',(1.,0.,0.));
#17079=DIRECTION('center_axis',(0.,1.,0.));
#17080=DIRECTION('ref_axis',(1.,0.,0.));
#17081=DIRECTION('',(0.,-1.,0.));
#17082=DIRECTION('center_axis',(0.,-1.,0.));
#17083=DIRECTION('ref_axis',(1.,0.,0.));
#17084=DIRECTION('center_axis',(0.,1.,0.));
#17085=DIRECTION('ref_axis',(1.,0.,0.));
#17086=DIRECTION('',(0.,-1.,0.));
#17087=DIRECTION('',(0.,1.,0.));
#17088=DIRECTION('center_axis',(0.951056516295154,0.,0.309016994374948));
#17089=DIRECTION('ref_axis',(0.309016994374948,0.,-0.951056516295154));
#17090=DIRECTION('',(0.309016994374948,0.,-0.951056516295154));
#17091=DIRECTION('',(0.,1.,0.));
#17092=DIRECTION('',(0.,1.,0.));
#17093=DIRECTION('center_axis',(0.,1.,0.));
#17094=DIRECTION('ref_axis',(1.,0.,0.));
#17095=DIRECTION('center_axis',(0.,1.,0.));
#17096=DIRECTION('ref_axis',(1.,0.,0.));
#17097=DIRECTION('',(0.,-1.,0.));
#17098=DIRECTION('',(0.,1.,0.));
#17099=DIRECTION('center_axis',(0.809016994374947,0.,0.587785252292473));
#17100=DIRECTION('ref_axis',(0.587785252292473,0.,-0.809016994374947));
#17101=DIRECTION('',(0.587785252292473,0.,-0.809016994374947));
#17102=DIRECTION('',(0.,1.,0.));
#17103=DIRECTION('',(0.,1.,0.));
#17104=DIRECTION('center_axis',(0.,1.,0.));
#17105=DIRECTION('ref_axis',(1.,0.,0.));
#17106=DIRECTION('center_axis',(0.,1.,0.));
#17107=DIRECTION('ref_axis',(1.,0.,0.));
#17108=DIRECTION('',(0.,-1.,0.));
#17109=DIRECTION('',(0.,1.,0.));
#17110=DIRECTION('center_axis',(0.587785252292473,0.,0.809016994374948));
#17111=DIRECTION('ref_axis',(0.809016994374948,0.,-0.587785252292473));
#17112=DIRECTION('',(0.809016994374948,0.,-0.587785252292473));
#17113=DIRECTION('',(0.,1.,0.));
#17114=DIRECTION('',(0.,1.,0.));
#17115=DIRECTION('center_axis',(0.,1.,0.));
#17116=DIRECTION('ref_axis',(1.,0.,0.));
#17117=DIRECTION('center_axis',(0.,1.,0.));
#17118=DIRECTION('ref_axis',(1.,0.,0.));
#17119=DIRECTION('',(0.,-1.,0.));
#17120=DIRECTION('',(0.,1.,0.));
#17121=DIRECTION('center_axis',(0.309016994374947,0.,0.951056516295154));
#17122=DIRECTION('ref_axis',(0.951056516295154,0.,-0.309016994374947));
#17123=DIRECTION('',(0.951056516295154,0.,-0.309016994374947));
#17124=DIRECTION('',(0.,1.,0.));
#17125=DIRECTION('',(0.,1.,0.));
#17126=DIRECTION('center_axis',(0.,1.,0.));
#17127=DIRECTION('ref_axis',(1.,0.,0.));
#17128=DIRECTION('center_axis',(0.,1.,0.));
#17129=DIRECTION('ref_axis',(1.,0.,0.));
#17130=DIRECTION('',(0.,-1.,0.));
#17131=DIRECTION('',(0.,1.,0.));
#17132=DIRECTION('center_axis',(-1.83697019872103E-16,0.,1.));
#17133=DIRECTION('ref_axis',(1.,0.,1.83697019872103E-16));
#17134=DIRECTION('',(1.,0.,1.83697019872103E-16));
#17135=DIRECTION('',(0.,1.,0.));
#17136=DIRECTION('',(0.,1.,0.));
#17137=DIRECTION('center_axis',(0.,1.,0.));
#17138=DIRECTION('ref_axis',(1.,0.,0.));
#17139=DIRECTION('center_axis',(0.,1.,0.));
#17140=DIRECTION('ref_axis',(1.,0.,0.));
#17141=DIRECTION('',(0.,-1.,0.));
#17142=DIRECTION('',(0.,1.,0.));
#17143=DIRECTION('center_axis',(-0.309016994374948,0.,0.951056516295154));
#17144=DIRECTION('ref_axis',(0.951056516295154,0.,0.309016994374948));
#17145=DIRECTION('',(0.951056516295154,0.,0.309016994374948));
#17146=DIRECTION('',(0.,1.,0.));
#17147=DIRECTION('',(0.,1.,0.));
#17148=DIRECTION('center_axis',(0.,1.,0.));
#17149=DIRECTION('ref_axis',(1.,0.,0.));
#17150=DIRECTION('center_axis',(0.,1.,0.));
#17151=DIRECTION('ref_axis',(1.,0.,0.));
#17152=DIRECTION('',(0.,-1.,0.));
#17153=DIRECTION('',(0.,1.,0.));
#17154=DIRECTION('center_axis',(-0.587785252292473,0.,0.809016994374947));
#17155=DIRECTION('ref_axis',(0.809016994374947,0.,0.587785252292473));
#17156=DIRECTION('',(0.809016994374947,0.,0.587785252292473));
#17157=DIRECTION('',(0.,1.,0.));
#17158=DIRECTION('',(0.,1.,0.));
#17159=DIRECTION('center_axis',(0.,1.,0.));
#17160=DIRECTION('ref_axis',(1.,0.,0.));
#17161=DIRECTION('center_axis',(0.,1.,0.));
#17162=DIRECTION('ref_axis',(1.,0.,0.));
#17163=DIRECTION('',(0.,-1.,0.));
#17164=DIRECTION('',(0.,1.,0.));
#17165=DIRECTION('center_axis',(-0.809016994374948,0.,0.587785252292473));
#17166=DIRECTION('ref_axis',(0.587785252292473,0.,0.809016994374948));
#17167=DIRECTION('',(0.587785252292473,0.,0.809016994374948));
#17168=DIRECTION('',(0.,1.,0.));
#17169=DIRECTION('',(0.,1.,0.));
#17170=DIRECTION('center_axis',(0.,1.,0.));
#17171=DIRECTION('ref_axis',(1.,0.,0.));
#17172=DIRECTION('center_axis',(0.,1.,0.));
#17173=DIRECTION('ref_axis',(1.,0.,0.));
#17174=DIRECTION('',(0.,-1.,0.));
#17175=DIRECTION('',(0.,1.,0.));
#17176=DIRECTION('center_axis',(-0.951056516295154,0.,0.309016994374947));
#17177=DIRECTION('ref_axis',(0.309016994374947,0.,0.951056516295154));
#17178=DIRECTION('',(0.309016994374947,0.,0.951056516295154));
#17179=DIRECTION('',(0.,1.,0.));
#17180=DIRECTION('',(0.,1.,0.));
#17181=DIRECTION('center_axis',(0.,1.,0.));
#17182=DIRECTION('ref_axis',(1.,0.,0.));
#17183=DIRECTION('center_axis',(0.,1.,0.));
#17184=DIRECTION('ref_axis',(1.,0.,0.));
#17185=DIRECTION('',(0.,-1.,0.));
#17186=DIRECTION('',(0.,1.,0.));
#17187=DIRECTION('center_axis',(-1.,0.,-1.22464679914735E-16));
#17188=DIRECTION('ref_axis',(-1.22464679914735E-16,0.,1.));
#17189=DIRECTION('',(-1.22464679914735E-16,0.,1.));
#17190=DIRECTION('',(0.,1.,0.));
#17191=DIRECTION('',(0.,1.,0.));
#17192=DIRECTION('center_axis',(0.,1.,0.));
#17193=DIRECTION('ref_axis',(1.,0.,0.));
#17194=DIRECTION('center_axis',(0.,1.,0.));
#17195=DIRECTION('ref_axis',(1.,0.,0.));
#17196=DIRECTION('',(0.,-1.,0.));
#17197=DIRECTION('',(0.,1.,0.));
#17198=DIRECTION('center_axis',(-0.951056516295154,0.,-0.309016994374948));
#17199=DIRECTION('ref_axis',(-0.309016994374948,0.,0.951056516295154));
#17200=DIRECTION('',(-0.309016994374948,0.,0.951056516295154));
#17201=DIRECTION('',(0.,1.,0.));
#17202=DIRECTION('',(0.,1.,0.));
#17203=DIRECTION('center_axis',(0.,1.,0.));
#17204=DIRECTION('ref_axis',(1.,0.,0.));
#17205=DIRECTION('center_axis',(0.,1.,0.));
#17206=DIRECTION('ref_axis',(1.,0.,0.));
#17207=DIRECTION('',(0.,-1.,0.));
#17208=DIRECTION('',(0.,1.,0.));
#17209=DIRECTION('center_axis',(-0.809016994374947,0.,-0.587785252292473));
#17210=DIRECTION('ref_axis',(-0.587785252292473,0.,0.809016994374947));
#17211=DIRECTION('',(-0.587785252292473,0.,0.809016994374947));
#17212=DIRECTION('',(0.,1.,0.));
#17213=DIRECTION('',(0.,1.,0.));
#17214=DIRECTION('center_axis',(0.,1.,0.));
#17215=DIRECTION('ref_axis',(1.,0.,0.));
#17216=DIRECTION('center_axis',(0.,1.,0.));
#17217=DIRECTION('ref_axis',(1.,0.,0.));
#17218=DIRECTION('',(0.,-1.,0.));
#17219=DIRECTION('',(0.,1.,0.));
#17220=DIRECTION('center_axis',(-0.587785252292473,0.,-0.809016994374948));
#17221=DIRECTION('ref_axis',(-0.809016994374948,0.,0.587785252292473));
#17222=DIRECTION('',(-0.809016994374948,0.,0.587785252292473));
#17223=DIRECTION('',(0.,1.,0.));
#17224=DIRECTION('',(0.,1.,0.));
#17225=DIRECTION('center_axis',(0.,1.,0.));
#17226=DIRECTION('ref_axis',(1.,0.,0.));
#17227=DIRECTION('center_axis',(0.,1.,0.));
#17228=DIRECTION('ref_axis',(1.,0.,0.));
#17229=DIRECTION('',(0.,-1.,0.));
#17230=DIRECTION('',(0.,1.,0.));
#17231=DIRECTION('center_axis',(-0.309016994374947,0.,-0.951056516295154));
#17232=DIRECTION('ref_axis',(-0.951056516295154,0.,0.309016994374947));
#17233=DIRECTION('',(-0.951056516295154,0.,0.309016994374947));
#17234=DIRECTION('',(0.,1.,0.));
#17235=DIRECTION('',(0.,1.,0.));
#17236=DIRECTION('center_axis',(0.,1.,0.));
#17237=DIRECTION('ref_axis',(1.,0.,0.));
#17238=DIRECTION('center_axis',(0.,1.,0.));
#17239=DIRECTION('ref_axis',(1.,0.,0.));
#17240=DIRECTION('',(0.,-1.,0.));
#17241=DIRECTION('',(0.,1.,0.));
#17242=DIRECTION('center_axis',(6.12323399573677E-17,0.,-1.));
#17243=DIRECTION('ref_axis',(-1.,0.,-6.12323399573677E-17));
#17244=DIRECTION('',(-1.,0.,-6.12323399573677E-17));
#17245=DIRECTION('',(0.,1.,0.));
#17246=DIRECTION('',(0.,1.,0.));
#17247=DIRECTION('center_axis',(0.,1.,0.));
#17248=DIRECTION('ref_axis',(1.,0.,0.));
#17249=DIRECTION('center_axis',(0.,1.,0.));
#17250=DIRECTION('ref_axis',(1.,0.,0.));
#17251=DIRECTION('',(0.,-1.,0.));
#17252=DIRECTION('',(0.,1.,0.));
#17253=DIRECTION('center_axis',(0.309016994374948,0.,-0.951056516295154));
#17254=DIRECTION('ref_axis',(-0.951056516295154,0.,-0.309016994374948));
#17255=DIRECTION('',(-0.951056516295154,0.,-0.309016994374948));
#17256=DIRECTION('',(0.,1.,0.));
#17257=DIRECTION('',(0.,1.,0.));
#17258=DIRECTION('center_axis',(0.,1.,0.));
#17259=DIRECTION('ref_axis',(1.,0.,0.));
#17260=DIRECTION('center_axis',(0.,1.,0.));
#17261=DIRECTION('ref_axis',(1.,0.,0.));
#17262=DIRECTION('',(0.,-1.,0.));
#17263=DIRECTION('',(0.,1.,0.));
#17264=DIRECTION('center_axis',(0.587785252292473,0.,-0.809016994374947));
#17265=DIRECTION('ref_axis',(-0.809016994374947,0.,-0.587785252292473));
#17266=DIRECTION('',(-0.809016994374947,0.,-0.587785252292473));
#17267=DIRECTION('',(0.,1.,0.));
#17268=DIRECTION('',(0.,1.,0.));
#17269=DIRECTION('center_axis',(0.,1.,0.));
#17270=DIRECTION('ref_axis',(1.,0.,0.));
#17271=DIRECTION('center_axis',(0.,1.,0.));
#17272=DIRECTION('ref_axis',(1.,0.,0.));
#17273=DIRECTION('',(0.,-1.,0.));
#17274=DIRECTION('',(0.,1.,0.));
#17275=DIRECTION('center_axis',(0.809016994374947,0.,-0.587785252292473));
#17276=DIRECTION('ref_axis',(-0.587785252292473,0.,-0.809016994374947));
#17277=DIRECTION('',(-0.587785252292473,0.,-0.809016994374947));
#17278=DIRECTION('',(0.,1.,0.));
#17279=DIRECTION('',(0.,1.,0.));
#17280=DIRECTION('center_axis',(0.,1.,0.));
#17281=DIRECTION('ref_axis',(1.,0.,0.));
#17282=DIRECTION('center_axis',(0.,1.,0.));
#17283=DIRECTION('ref_axis',(1.,0.,0.));
#17284=DIRECTION('',(0.,-1.,0.));
#17285=DIRECTION('',(0.,1.,0.));
#17286=DIRECTION('center_axis',(0.951056516295154,0.,-0.309016994374947));
#17287=DIRECTION('ref_axis',(-0.309016994374947,0.,-0.951056516295154));
#17288=DIRECTION('',(-0.309016994374947,0.,-0.951056516295154));
#17289=DIRECTION('',(0.,1.,0.));
#17290=DIRECTION('',(0.,1.,0.));
#17291=DIRECTION('center_axis',(0.,1.,0.));
#17292=DIRECTION('ref_axis',(1.,0.,0.));
#17293=DIRECTION('center_axis',(0.,1.,0.));
#17294=DIRECTION('ref_axis',(1.,0.,0.));
#17295=DIRECTION('',(0.,-1.,0.));
#17296=DIRECTION('',(0.,1.,0.));
#17297=DIRECTION('center_axis',(1.,0.,0.));
#17298=DIRECTION('ref_axis',(0.,0.,-1.));
#17299=DIRECTION('',(0.,0.,-1.));
#17300=DIRECTION('',(0.,1.,0.));
#17301=DIRECTION('',(0.,1.,0.));
#17302=DIRECTION('center_axis',(0.,1.,0.));
#17303=DIRECTION('ref_axis',(1.,0.,0.));
#17304=DIRECTION('center_axis',(0.,1.,0.));
#17305=DIRECTION('ref_axis',(1.,0.,0.));
#17306=DIRECTION('center_axis',(0.,1.,0.));
#17307=DIRECTION('ref_axis',(1.,0.,0.));
#17308=DIRECTION('axis',(0.,0.,1.));
#17309=DIRECTION('refdir',(1.,0.,0.));
#17310=DIRECTION('center_axis',(0.,1.,0.));
#17311=DIRECTION('ref_axis',(1.,0.,0.));
#17312=DIRECTION('center_axis',(0.,-1.,0.));
#17313=DIRECTION('ref_axis',(1.,0.,0.));
#17314=DIRECTION('',(0.,-1.,0.));
#17315=DIRECTION('center_axis',(0.,-1.,0.));
#17316=DIRECTION('ref_axis',(1.,0.,0.));
#17317=DIRECTION('center_axis',(0.,1.,0.));
#17318=DIRECTION('ref_axis',(1.,0.,0.));
#17319=DIRECTION('center_axis',(0.,1.,0.));
#17320=DIRECTION('ref_axis',(1.,0.,0.));
#17321=DIRECTION('',(0.,-1.,0.));
#17322=DIRECTION('center_axis',(0.,1.,0.));
#17323=DIRECTION('ref_axis',(1.,0.,0.));
#17324=DIRECTION('center_axis',(0.,1.,0.));
#17325=DIRECTION('ref_axis',(1.,0.,0.));
#17326=DIRECTION('center_axis',(0.,1.,0.));
#17327=DIRECTION('ref_axis',(1.,0.,0.));
#17328=DIRECTION('axis',(0.,0.,1.));
#17329=DIRECTION('refdir',(1.,0.,0.));
#17330=DIRECTION('center_axis',(0.,1.,0.));
#17331=DIRECTION('ref_axis',(0.,0.,1.));
#17332=DIRECTION('center_axis',(0.,-1.,0.));
#17333=DIRECTION('ref_axis',(1.,0.,0.));
#17334=DIRECTION('center_axis',(0.,-1.,0.));
#17335=DIRECTION('ref_axis',(1.,0.,0.));
#17336=DIRECTION('center_axis',(0.,-1.,0.));
#17337=DIRECTION('ref_axis',(1.,0.,0.));
#17338=DIRECTION('',(0.707106781186548,0.707106781186547,8.65956056235494E-17));
#17339=DIRECTION('center_axis',(0.,-1.,0.));
#17340=DIRECTION('ref_axis',(1.,0.,0.));
#17341=DIRECTION('center_axis',(0.,-1.,0.));
#17342=DIRECTION('ref_axis',(1.,0.,0.));
#17343=DIRECTION('',(0.,1.,0.));
#17344=DIRECTION('center_axis',(0.,1.,0.));
#17345=DIRECTION('ref_axis',(1.,0.,0.));
#17346=DIRECTION('center_axis',(0.,-1.,0.));
#17347=DIRECTION('ref_axis',(1.,0.,0.));
#17348=DIRECTION('',(-0.707106781186547,0.707106781186548,-8.65956056235493E-17));
#17349=DIRECTION('center_axis',(0.,-1.,0.));
#17350=DIRECTION('ref_axis',(0.,0.,-1.));
#17351=DIRECTION('center_axis',(0.,-1.,0.));
#17352=DIRECTION('ref_axis',(1.,0.,0.));
#17353=DIRECTION('center_axis',(0.,1.,0.));
#17354=DIRECTION('ref_axis',(1.,0.,0.));
#17355=DIRECTION('center_axis',(0.,1.,0.));
#17356=DIRECTION('ref_axis',(1.,0.,0.));
#17357=DIRECTION('',(-0.447213595499958,0.894427190999916,-5.47678698264203E-17));
#17358=DIRECTION('center_axis',(0.,-1.,0.));
#17359=DIRECTION('ref_axis',(1.,0.,0.));
#17360=DIRECTION('center_axis',(0.,1.,0.));
#17361=DIRECTION('ref_axis',(1.,0.,0.));
#17362=DIRECTION('',(0.,1.,0.));
#17363=DIRECTION('center_axis',(0.,1.,0.));
#17364=DIRECTION('ref_axis',(1.,0.,0.));
#17365=DIRECTION('center_axis',(0.,-1.,0.));
#17366=DIRECTION('ref_axis',(1.,0.,0.));
#17367=DIRECTION('',(-0.707106781186547,0.707106781186548,-8.65956056235493E-17));
#17368=DIRECTION('center_axis',(0.,-1.,0.));
#17369=DIRECTION('ref_axis',(0.,0.,-1.));
#17370=DIRECTION('center_axis',(0.866025403784439,0.,-0.5));
#17371=DIRECTION('ref_axis',(0.5,0.,0.866025403784439));
#17372=DIRECTION('',(-0.5,0.,-0.866025403784439));
#17373=DIRECTION('',(0.,-1.,0.));
#17374=DIRECTION('',(0.5,0.,0.866025403784439));
#17375=DIRECTION('',(0.,-1.,0.));
#17376=DIRECTION('center_axis',(1.92296268638356E-16,0.,-1.));
#17377=DIRECTION('ref_axis',(1.,0.,1.92296268638356E-16));
#17378=DIRECTION('',(-1.,0.,-1.92296268638356E-16));
#17379=DIRECTION('',(0.,-1.,0.));
#17380=DIRECTION('',(1.,0.,1.92296268638356E-16));
#17381=DIRECTION('center_axis',(-0.866025403784439,0.,-0.5));
#17382=DIRECTION('ref_axis',(0.5,0.,-0.866025403784439));
#17383=DIRECTION('',(-0.5,0.,0.866025403784438));
#17384=DIRECTION('',(0.,-1.,0.));
#17385=DIRECTION('',(0.5,0.,-0.866025403784438));
#17386=DIRECTION('center_axis',(-0.866025403784439,0.,0.5));
#17387=DIRECTION('ref_axis',(-0.5,0.,-0.866025403784439));
#17388=DIRECTION('',(0.5,0.,0.866025403784439));
#17389=DIRECTION('',(0.,-1.,0.));
#17390=DIRECTION('',(-0.5,0.,-0.866025403784439));
#17391=DIRECTION('center_axis',(-1.92296268638356E-16,0.,1.));
#17392=DIRECTION('ref_axis',(-1.,0.,-1.92296268638356E-16));
#17393=DIRECTION('',(1.,0.,1.92296268638356E-16));
#17394=DIRECTION('',(0.,-1.,0.));
#17395=DIRECTION('',(-1.,0.,-1.92296268638356E-16));
#17396=DIRECTION('center_axis',(0.866025403784439,0.,0.5));
#17397=DIRECTION('ref_axis',(-0.5,0.,0.866025403784439));
#17398=DIRECTION('',(0.5,0.,-0.866025403784439));
#17399=DIRECTION('',(-0.5,0.,0.866025403784439));
#17400=DIRECTION('center_axis',(0.,1.,0.));
#17401=DIRECTION('ref_axis',(1.,0.,0.));
#17402=DIRECTION('center_axis',(0.,-1.,0.));
#17403=DIRECTION('ref_axis',(0.,0.,-1.));
#17404=DIRECTION('axis',(0.,0.,1.));
#17405=DIRECTION('refdir',(1.,0.,0.));
#17406=DIRECTION('center_axis',(0.,1.,0.));
#17407=DIRECTION('ref_axis',(0.,0.,1.));
#17408=DIRECTION('center_axis',(0.,-1.,0.));
#17409=DIRECTION('ref_axis',(1.,0.,0.));
#17410=DIRECTION('center_axis',(0.,-1.,0.));
#17411=DIRECTION('ref_axis',(1.,0.,0.));
#17412=DIRECTION('center_axis',(0.,-1.,0.));
#17413=DIRECTION('ref_axis',(1.,0.,0.));
#17414=DIRECTION('',(0.707106781186547,0.707106781186548,8.65956056235493E-17));
#17415=DIRECTION('center_axis',(0.,-1.,0.));
#17416=DIRECTION('ref_axis',(1.,0.,0.));
#17417=DIRECTION('center_axis',(0.,-1.,0.));
#17418=DIRECTION('ref_axis',(1.,0.,0.));
#17419=DIRECTION('',(0.,1.,0.));
#17420=DIRECTION('center_axis',(0.,1.,0.));
#17421=DIRECTION('ref_axis',(1.,0.,0.));
#17422=DIRECTION('center_axis',(0.,-1.,0.));
#17423=DIRECTION('ref_axis',(1.,0.,0.));
#17424=DIRECTION('',(-0.707106781186547,0.707106781186548,-8.65956056235493E-17));
#17425=DIRECTION('center_axis',(0.,-1.,0.));
#17426=DIRECTION('ref_axis',(0.,0.,-1.));
#17427=DIRECTION('center_axis',(0.,-1.,0.));
#17428=DIRECTION('ref_axis',(1.,0.,0.));
#17429=DIRECTION('center_axis',(0.,1.,0.));
#17430=DIRECTION('ref_axis',(1.,0.,0.));
#17431=DIRECTION('center_axis',(0.,1.,0.));
#17432=DIRECTION('ref_axis',(1.,0.,0.));
#17433=DIRECTION('',(-0.447213595499958,0.894427190999916,-5.47678698264203E-17));
#17434=DIRECTION('center_axis',(0.,-1.,0.));
#17435=DIRECTION('ref_axis',(1.,0.,0.));
#17436=DIRECTION('center_axis',(0.,1.,0.));
#17437=DIRECTION('ref_axis',(1.,0.,0.));
#17438=DIRECTION('',(0.,1.,0.));
#17439=DIRECTION('center_axis',(0.,1.,0.));
#17440=DIRECTION('ref_axis',(1.,0.,0.));
#17441=DIRECTION('center_axis',(0.,-1.,0.));
#17442=DIRECTION('ref_axis',(1.,0.,0.));
#17443=DIRECTION('',(-0.707106781186547,0.707106781186548,-8.65956056235493E-17));
#17444=DIRECTION('center_axis',(0.,-1.,0.));
#17445=DIRECTION('ref_axis',(0.,0.,-1.));
#17446=DIRECTION('center_axis',(0.866025403784439,0.,-0.5));
#17447=DIRECTION('ref_axis',(0.5,0.,0.866025403784439));
#17448=DIRECTION('',(-0.5,0.,-0.866025403784439));
#17449=DIRECTION('',(0.,-1.,0.));
#17450=DIRECTION('',(0.5,0.,0.866025403784439));
#17451=DIRECTION('',(0.,-1.,0.));
#17452=DIRECTION('center_axis',(1.60246890531964E-16,0.,-1.));
#17453=DIRECTION('ref_axis',(1.,0.,1.60246890531964E-16));
#17454=DIRECTION('',(-1.,0.,-1.60246890531964E-16));
#17455=DIRECTION('',(0.,-1.,0.));
#17456=DIRECTION('',(1.,0.,1.60246890531964E-16));
#17457=DIRECTION('center_axis',(-0.866025403784439,0.,-0.5));
#17458=DIRECTION('ref_axis',(0.5,0.,-0.866025403784439));
#17459=DIRECTION('',(-0.5,0.,0.866025403784439));
#17460=DIRECTION('',(0.,-1.,0.));
#17461=DIRECTION('',(0.5,0.,-0.866025403784439));
#17462=DIRECTION('center_axis',(-0.866025403784439,0.,0.5));
#17463=DIRECTION('ref_axis',(-0.5,0.,-0.866025403784439));
#17464=DIRECTION('',(0.5,0.,0.866025403784439));
#17465=DIRECTION('',(0.,-1.,0.));
#17466=DIRECTION('',(-0.5,0.,-0.866025403784439));
#17467=DIRECTION('center_axis',(-1.60246890531964E-16,0.,1.));
#17468=DIRECTION('ref_axis',(-1.,0.,-1.60246890531964E-16));
#17469=DIRECTION('',(1.,0.,1.60246890531964E-16));
#17470=DIRECTION('',(0.,-1.,0.));
#17471=DIRECTION('',(-1.,0.,-1.60246890531964E-16));
#17472=DIRECTION('center_axis',(0.866025403784439,0.,0.5));
#17473=DIRECTION('ref_axis',(-0.5,0.,0.866025403784439));
#17474=DIRECTION('',(0.5,0.,-0.866025403784439));
#17475=DIRECTION('',(-0.5,0.,0.866025403784439));
#17476=DIRECTION('center_axis',(0.,1.,0.));
#17477=DIRECTION('ref_axis',(1.,0.,0.));
#17478=DIRECTION('center_axis',(0.,-1.,0.));
#17479=DIRECTION('ref_axis',(0.,0.,-1.));
#17480=DIRECTION('',(0.,0.,1.));
#17481=DIRECTION('',(1.,0.,0.));
#17482=DIRECTION('',(0.,0.,1.));
#17483=DIRECTION('',(1.,0.,0.));
#17484=DIRECTION('',(0.,0.,1.));
#17485=DIRECTION('',(1.,0.,0.));
#17486=DIRECTION('',(0.,0.,1.));
#17487=DIRECTION('',(1.,0.,0.));
#17488=DIRECTION('',(0.,0.,1.));
#17489=DIRECTION('',(1.,0.,0.));
#17490=DIRECTION('',(0.,0.,1.));
#17491=DIRECTION('',(1.,0.,0.));
#17492=DIRECTION('',(0.,0.,1.));
#17493=DIRECTION('',(1.,0.,0.));
#17494=DIRECTION('',(0.,0.,1.));
#17495=DIRECTION('',(1.,0.,0.));
#17496=DIRECTION('',(0.,0.,1.));
#17497=DIRECTION('',(1.,0.,0.));
#17498=DIRECTION('',(0.,0.,1.));
#17499=DIRECTION('',(1.,0.,0.));
#17500=DIRECTION('',(0.,0.,1.));
#17501=DIRECTION('',(1.,0.,0.));
#17502=DIRECTION('',(0.,0.,1.));
#17503=DIRECTION('',(1.,0.,0.));
#17504=DIRECTION('',(0.,0.,1.));
#17505=DIRECTION('',(1.,0.,0.));
#17506=DIRECTION('',(0.,0.,1.));
#17507=DIRECTION('',(1.,0.,0.));
#17508=DIRECTION('',(0.,0.,1.));
#17509=DIRECTION('',(1.,0.,0.));
#17510=DIRECTION('',(0.,-1.,2.22044604925031E-16));
#17511=DIRECTION('',(1.,0.,0.));
#17512=DIRECTION('',(0.,-1.,2.22044604925031E-16));
#17513=DIRECTION('',(1.,0.,0.));
#17514=DIRECTION('',(0.,-1.,2.22044604925031E-16));
#17515=DIRECTION('',(1.,0.,0.));
#17516=DIRECTION('',(0.,-1.,2.22044604925031E-16));
#17517=DIRECTION('',(1.,0.,0.));
#17518=DIRECTION('',(0.,-1.,2.22044604925031E-16));
#17519=DIRECTION('',(1.,0.,0.));
#17520=DIRECTION('',(0.,-1.,2.22044604925031E-16));
#17521=DIRECTION('',(1.,0.,0.));
#17522=DIRECTION('',(0.,-1.,2.22044604925031E-16));
#17523=DIRECTION('',(1.,0.,0.));
#17524=DIRECTION('',(0.,-1.,2.22044604925031E-16));
#17525=DIRECTION('',(1.,0.,0.));
#17526=DIRECTION('',(0.,-1.,2.22044604925031E-16));
#17527=DIRECTION('',(1.,0.,0.));
#17528=DIRECTION('',(0.,-1.,2.22044604925031E-16));
#17529=DIRECTION('',(1.,0.,0.));
#17530=DIRECTION('',(0.,-1.,2.22044604925031E-16));
#17531=DIRECTION('',(1.,0.,0.));
#17532=DIRECTION('',(0.,-1.,2.22044604925031E-16));
#17533=DIRECTION('',(1.,0.,0.));
#17534=DIRECTION('',(0.,0.,1.));
#17535=DIRECTION('',(1.,0.,0.));
#17536=DIRECTION('',(0.,0.,1.));
#17537=DIRECTION('',(-1.,1.22464679914735E-16,0.));
#17538=DIRECTION('',(0.,0.,1.));
#17539=DIRECTION('',(-1.,1.22464679914735E-16,0.));
#17540=DIRECTION('',(0.,0.,1.));
#17541=DIRECTION('',(-1.,1.22464679914735E-16,0.));
#17542=DIRECTION('',(0.,0.,1.));
#17543=DIRECTION('',(-1.,1.22464679914735E-16,0.));
#17544=DIRECTION('',(0.,0.,1.));
#17545=DIRECTION('',(1.,0.,0.));
#17546=DIRECTION('',(0.,0.,1.));
#17547=DIRECTION('',(1.,0.,0.));
#17548=DIRECTION('',(0.,0.,1.));
#17549=DIRECTION('',(1.,0.,0.));
#17550=DIRECTION('',(0.,0.,1.));
#17551=DIRECTION('',(1.,0.,0.));
#17552=DIRECTION('',(0.,-1.,2.22044604925031E-16));
#17553=DIRECTION('',(1.,0.,0.));
#17554=DIRECTION('',(0.,-1.,2.22044604925031E-16));
#17555=DIRECTION('',(1.,0.,0.));
#17556=DIRECTION('',(0.,0.,1.));
#17557=DIRECTION('',(1.,0.,0.));
#17558=DIRECTION('',(0.,0.,1.));
#17559=DIRECTION('',(-1.,1.22464679914735E-16,0.));
#17560=DIRECTION('',(0.,0.,1.));
#17561=DIRECTION('',(-1.,1.22464679914735E-16,0.));
#17562=DIRECTION('',(0.,0.,1.));
#17563=DIRECTION('',(-1.,1.22464679914735E-16,0.));
#17564=DIRECTION('',(0.,0.,1.));
#17565=DIRECTION('',(-1.,1.22464679914735E-16,0.));
#17566=DIRECTION('',(0.,0.,1.));
#17567=DIRECTION('',(1.,0.,0.));
#17568=DIRECTION('',(0.,0.,1.));
#17569=DIRECTION('',(1.,0.,0.));
#17570=DIRECTION('',(0.,0.,1.));
#17571=DIRECTION('',(1.,0.,0.));
#17572=DIRECTION('',(0.,0.,1.));
#17573=DIRECTION('',(1.,0.,0.));
#17574=DIRECTION('',(0.,0.,1.));
#17575=DIRECTION('',(1.,0.,0.));
#17576=DIRECTION('',(0.,0.,1.));
#17577=DIRECTION('',(1.,0.,0.));
#17578=DIRECTION('',(0.,0.,1.));
#17579=DIRECTION('',(1.,0.,0.));
#17580=DIRECTION('',(0.,0.,1.));
#17581=DIRECTION('',(1.,0.,0.));
#17582=DIRECTION('',(0.,0.,1.));
#17583=DIRECTION('',(1.,0.,0.));
#17584=DIRECTION('',(0.,0.,1.));
#17585=DIRECTION('',(1.,0.,0.));
#17586=DIRECTION('',(0.,0.,1.));
#17587=DIRECTION('',(1.,0.,0.));
#17588=DIRECTION('',(0.,0.,1.));
#17589=DIRECTION('',(1.,0.,0.));
#17590=DIRECTION('',(0.,0.,1.));
#17591=DIRECTION('',(1.,0.,0.));
#17592=DIRECTION('',(0.,0.,1.));
#17593=DIRECTION('',(1.,0.,0.));
#17594=DIRECTION('',(0.,0.,1.));
#17595=DIRECTION('',(1.,0.,0.));
#17596=DIRECTION('',(-1.,0.,2.22044604925031E-16));
#17597=DIRECTION('',(2.22044604925031E-16,0.,1.));
#17598=DIRECTION('',(0.,0.,1.));
#17599=DIRECTION('',(1.,0.,0.));
#17600=DIRECTION('',(0.,0.,1.));
#17601=DIRECTION('',(1.,0.,0.));
#17602=DIRECTION('',(0.,0.,1.));
#17603=DIRECTION('',(-1.,1.22464679914735E-16,0.));
#17604=DIRECTION('',(0.,0.,1.));
#17605=DIRECTION('',(1.,0.,0.));
#17606=DIRECTION('axis',(0.,0.,1.));
#17607=DIRECTION('refdir',(1.,0.,0.));
#17608=DIRECTION('axis',(0.,0.,1.));
#17609=DIRECTION('refdir',(1.,0.,0.));
#17610=DIRECTION('center_axis',(0.,1.,0.));
#17611=DIRECTION('ref_axis',(1.,0.,0.));
#17612=DIRECTION('center_axis',(0.,-1.,0.));
#17613=DIRECTION('ref_axis',(1.,0.,0.));
#17614=DIRECTION('',(0.,-1.,0.));
#17615=DIRECTION('center_axis',(0.,-1.,0.));
#17616=DIRECTION('ref_axis',(1.,0.,0.));
#17617=DIRECTION('center_axis',(0.,1.,0.));
#17618=DIRECTION('ref_axis',(1.,0.,0.));
#17619=DIRECTION('center_axis',(0.,1.,0.));
#17620=DIRECTION('ref_axis',(1.,0.,0.));
#17621=DIRECTION('',(0.,-1.,0.));
#17622=DIRECTION('center_axis',(0.,1.,0.));
#17623=DIRECTION('ref_axis',(1.,0.,0.));
#17624=DIRECTION('center_axis',(0.,1.,0.));
#17625=DIRECTION('ref_axis',(1.,0.,0.));
#17626=DIRECTION('center_axis',(0.,1.,0.));
#17627=DIRECTION('ref_axis',(1.,0.,0.));
#17628=DIRECTION('',(0.,0.,1.));
#17629=DIRECTION('',(1.,0.,0.));
#17630=DIRECTION('',(0.,0.,1.));
#17631=DIRECTION('',(1.,0.,0.));
#17632=DIRECTION('',(0.,0.,1.));
#17633=DIRECTION('',(1.,0.,0.));
#17634=DIRECTION('',(0.,0.,1.));
#17635=DIRECTION('',(1.,0.,0.));
#17636=DIRECTION('',(0.,0.,1.));
#17637=DIRECTION('',(1.,0.,0.));
#17638=CARTESIAN_POINT('',(0.,0.,0.));
#17639=CARTESIAN_POINT('',(0.,0.,0.));
#17640=CARTESIAN_POINT('',(0.,0.,0.));
#17641=CARTESIAN_POINT('Origin',(-6.05,3.,-0.1));
#17642=CARTESIAN_POINT('',(-6.215,3.,0.));
#17643=CARTESIAN_POINT('Origin',(-6.05,3.,0.));
#17644=CARTESIAN_POINT('',(-6.215,3.,1.));
#17645=CARTESIAN_POINT('',(-6.215,3.,-0.1));
#17646=CARTESIAN_POINT('Origin',(-6.05,3.,1.));
#17647=CARTESIAN_POINT('Origin',(-0.45,3.,-0.1));
#17648=CARTESIAN_POINT('',(-0.615,3.,0.));
#17649=CARTESIAN_POINT('Origin',(-0.45,3.,0.));
#17650=CARTESIAN_POINT('',(-0.615,3.,1.));
#17651=CARTESIAN_POINT('',(-0.615,3.,-0.1));
#17652=CARTESIAN_POINT('Origin',(-0.45,3.,1.));
#17653=CARTESIAN_POINT('Origin',(-6.05,-3.,-0.1));
#17654=CARTESIAN_POINT('',(-6.215,-3.,0.));
#17655=CARTESIAN_POINT('Origin',(-6.05,-3.,0.));
#17656=CARTESIAN_POINT('',(-6.215,-3.,1.));
#17657=CARTESIAN_POINT('',(-6.215,-3.,-0.1));
#17658=CARTESIAN_POINT('Origin',(-6.05,-3.,1.));
#17659=CARTESIAN_POINT('Origin',(-0.45,-3.,-0.1));
#17660=CARTESIAN_POINT('',(-0.615,-3.,0.));
#17661=CARTESIAN_POINT('Origin',(-0.45,-3.,0.));
#17662=CARTESIAN_POINT('',(-0.615,-3.,1.));
#17663=CARTESIAN_POINT('',(-0.615,-3.,-0.1));
#17664=CARTESIAN_POINT('Origin',(-0.45,-3.,1.));
#17665=CARTESIAN_POINT('Origin',(1.,-1.8,-0.1));
#17666=CARTESIAN_POINT('',(0.835,-1.8,0.));
#17667=CARTESIAN_POINT('Origin',(1.,-1.8,0.));
#17668=CARTESIAN_POINT('',(0.835,-1.8,1.));
#17669=CARTESIAN_POINT('',(0.835,-1.8,-0.1));
#17670=CARTESIAN_POINT('Origin',(1.,-1.8,1.));
#17671=CARTESIAN_POINT('Origin',(1.,1.8,-0.1));
#17672=CARTESIAN_POINT('',(0.835,1.8,0.));
#17673=CARTESIAN_POINT('Origin',(1.,1.8,0.));
#17674=CARTESIAN_POINT('',(0.835,1.8,1.));
#17675=CARTESIAN_POINT('',(0.835,1.8,-0.1));
#17676=CARTESIAN_POINT('Origin',(1.,1.8,1.));
#17677=CARTESIAN_POINT('Origin',(7.,-3.2,-0.1));
#17678=CARTESIAN_POINT('',(6.79,-3.2,0.));
#17679=CARTESIAN_POINT('Origin',(7.,-3.2,0.));
#17680=CARTESIAN_POINT('',(6.79,-3.2,1.));
#17681=CARTESIAN_POINT('',(6.79,-3.2,-0.1));
#17682=CARTESIAN_POINT('Origin',(7.,-3.2,1.));
#17683=CARTESIAN_POINT('Origin',(4.,3.2,-0.1));
#17684=CARTESIAN_POINT('',(3.79,3.2,0.));
#17685=CARTESIAN_POINT('Origin',(4.,3.2,0.));
#17686=CARTESIAN_POINT('',(3.79,3.2,1.));
#17687=CARTESIAN_POINT('',(3.79,3.2,-0.1));
#17688=CARTESIAN_POINT('Origin',(4.,3.2,1.));
#17689=CARTESIAN_POINT('Origin',(4.,-3.2,-0.1));
#17690=CARTESIAN_POINT('',(3.79,-3.2,0.));
#17691=CARTESIAN_POINT('Origin',(4.,-3.2,0.));
#17692=CARTESIAN_POINT('',(3.79,-3.2,1.));
#17693=CARTESIAN_POINT('',(3.79,-3.2,-0.1));
#17694=CARTESIAN_POINT('Origin',(4.,-3.2,1.));
#17695=CARTESIAN_POINT('Origin',(7.,3.2,-0.1));
#17696=CARTESIAN_POINT('',(6.79,3.2,0.));
#17697=CARTESIAN_POINT('Origin',(7.,3.2,0.));
#17698=CARTESIAN_POINT('',(6.79,3.2,1.));
#17699=CARTESIAN_POINT('',(6.79,3.2,-0.1));
#17700=CARTESIAN_POINT('Origin',(7.,3.2,1.));
#17701=CARTESIAN_POINT('Origin',(10.,9.,0.));
#17702=CARTESIAN_POINT('',(10.,9.,0.));
#17703=CARTESIAN_POINT('',(-8.,9.,0.));
#17704=CARTESIAN_POINT('',(10.,9.,0.));
#17705=CARTESIAN_POINT('',(-8.,9.,1.));
#17706=CARTESIAN_POINT('',(-8.,9.,0.));
#17707=CARTESIAN_POINT('',(10.,9.,1.));
#17708=CARTESIAN_POINT('',(10.,9.,1.));
#17709=CARTESIAN_POINT('',(10.,9.,0.));
#17710=CARTESIAN_POINT('Origin',(10.,-9.,0.));
#17711=CARTESIAN_POINT('',(10.,-9.,0.));
#17712=CARTESIAN_POINT('',(10.,-9.,0.));
#17713=CARTESIAN_POINT('',(10.,-9.,1.));
#17714=CARTESIAN_POINT('',(10.,-9.,1.));
#17715=CARTESIAN_POINT('',(10.,-9.,0.));
#17716=CARTESIAN_POINT('Origin',(-8.,-9.,0.));
#17717=CARTESIAN_POINT('',(-8.,-9.,0.));
#17718=CARTESIAN_POINT('',(-8.,-9.,0.));
#17719=CARTESIAN_POINT('',(-8.,-9.,1.));
#17720=CARTESIAN_POINT('',(-8.,-9.,1.));
#17721=CARTESIAN_POINT('',(-8.,-9.,0.));
#17722=CARTESIAN_POINT('Origin',(-8.,9.,0.));
#17723=CARTESIAN_POINT('',(-8.,9.,0.));
#17724=CARTESIAN_POINT('',(-8.,9.,1.));
#17725=CARTESIAN_POINT('Origin',(1.,0.,1.));
#17726=CARTESIAN_POINT('Origin',(1.,0.,0.));
#17727=CARTESIAN_POINT('',(0.,0.,0.));
#17728=CARTESIAN_POINT('Origin',(-7.,9.,-0.8));
#17729=CARTESIAN_POINT('',(-7.,9.,-0.8));
#17730=CARTESIAN_POINT('',(-8.,9.,-0.8));
#17731=CARTESIAN_POINT('',(-7.,9.,-0.8));
#17732=CARTESIAN_POINT('',(-8.,9.,0.));
#17733=CARTESIAN_POINT('',(-8.,9.,-0.8));
#17734=CARTESIAN_POINT('',(-7.,9.,0.));
#17735=CARTESIAN_POINT('',(-7.,9.,0.));
#17736=CARTESIAN_POINT('',(-7.,9.,-0.8));
#17737=CARTESIAN_POINT('Origin',(-7.,-9.,-0.8));
#17738=CARTESIAN_POINT('',(-7.,-9.,-0.8));
#17739=CARTESIAN_POINT('',(-7.,-9.,-0.8));
#17740=CARTESIAN_POINT('',(-7.,-9.,0.));
#17741=CARTESIAN_POINT('',(-7.,-9.,0.));
#17742=CARTESIAN_POINT('',(-7.,-9.,-0.8));
#17743=CARTESIAN_POINT('Origin',(-8.,-9.,-0.8));
#17744=CARTESIAN_POINT('',(-8.,-9.,-0.8));
#17745=CARTESIAN_POINT('',(-8.,-9.,-0.8));
#17746=CARTESIAN_POINT('',(-8.,-9.,0.));
#17747=CARTESIAN_POINT('',(-8.,-9.,0.));
#17748=CARTESIAN_POINT('',(-8.,-9.,-0.8));
#17749=CARTESIAN_POINT('Origin',(-8.,9.,-0.8));
#17750=CARTESIAN_POINT('',(-8.,9.,-0.8));
#17751=CARTESIAN_POINT('',(-8.,9.,0.));
#17752=CARTESIAN_POINT('Origin',(-7.5,0.,0.));
#17753=CARTESIAN_POINT('Origin',(-7.5,0.,-0.8));
#17754=CARTESIAN_POINT('',(0.,0.,0.));
#17755=CARTESIAN_POINT('Origin',(10.,9.,-0.8));
#17756=CARTESIAN_POINT('',(10.,9.,-0.8));
#17757=CARTESIAN_POINT('',(9.,9.,-0.8));
#17758=CARTESIAN_POINT('',(10.,9.,-0.8));
#17759=CARTESIAN_POINT('',(9.,9.,0.));
#17760=CARTESIAN_POINT('',(9.,9.,-0.8));
#17761=CARTESIAN_POINT('',(10.,9.,0.));
#17762=CARTESIAN_POINT('',(10.,9.,0.));
#17763=CARTESIAN_POINT('',(10.,9.,-0.8));
#17764=CARTESIAN_POINT('Origin',(10.,-9.,-0.8));
#17765=CARTESIAN_POINT('',(10.,-9.,-0.8));
#17766=CARTESIAN_POINT('',(10.,-9.,-0.8));
#17767=CARTESIAN_POINT('',(10.,-9.,0.));
#17768=CARTESIAN_POINT('',(10.,-9.,0.));
#17769=CARTESIAN_POINT('',(10.,-9.,-0.8));
#17770=CARTESIAN_POINT('Origin',(9.,-9.,-0.8));
#17771=CARTESIAN_POINT('',(9.,-9.,-0.8));
#17772=CARTESIAN_POINT('',(9.,-9.,-0.8));
#17773=CARTESIAN_POINT('',(9.,-9.,0.));
#17774=CARTESIAN_POINT('',(9.,-9.,0.));
#17775=CARTESIAN_POINT('',(9.,-9.,-0.8));
#17776=CARTESIAN_POINT('Origin',(9.,9.,-0.8));
#17777=CARTESIAN_POINT('',(9.,9.,-0.8));
#17778=CARTESIAN_POINT('',(9.,9.,0.));
#17779=CARTESIAN_POINT('Origin',(9.5,0.,0.));
#17780=CARTESIAN_POINT('Origin',(9.5,0.,-0.8));
#17781=CARTESIAN_POINT('',(0.,0.,0.));
#17782=CARTESIAN_POINT('Origin',(2.4,-1.6,24.4));
#17783=CARTESIAN_POINT('',(2.235,-1.6,24.4));
#17784=CARTESIAN_POINT('Origin',(2.4,-1.6,24.4));
#17785=CARTESIAN_POINT('',(2.235,-1.6,25.));
#17786=CARTESIAN_POINT('',(2.235,-1.6,24.4));
#17787=CARTESIAN_POINT('Origin',(2.4,-1.6,25.));
#17788=CARTESIAN_POINT('Origin',(2.4,-1.6,24.4));
#17789=CARTESIAN_POINT('Origin',(2.4,1.6,24.4));
#17790=CARTESIAN_POINT('',(2.235,1.6,24.4));
#17791=CARTESIAN_POINT('Origin',(2.4,1.6,24.4));
#17792=CARTESIAN_POINT('',(2.235,1.6,25.));
#17793=CARTESIAN_POINT('',(2.235,1.6,24.4));
#17794=CARTESIAN_POINT('Origin',(2.4,1.6,25.));
#17795=CARTESIAN_POINT('Origin',(2.4,1.6,24.4));
#17796=CARTESIAN_POINT('Origin',(0.21,1.01,22.9));
#17797=CARTESIAN_POINT('',(-0.726238685697896,1.01,23.));
#17798=CARTESIAN_POINT('',(-0.726238685697896,1.01,25.));
#17799=CARTESIAN_POINT('',(-0.726238685697896,1.01,23.));
#17800=CARTESIAN_POINT('',(0.0305156009506911,1.01,23.));
#17801=CARTESIAN_POINT('',(1.98,1.01,23.));
#17802=CARTESIAN_POINT('',(0.0305156009506911,1.01,25.));
#17803=CARTESIAN_POINT('',(0.0305156009506911,1.01,22.9));
#17804=CARTESIAN_POINT('',(1.98,1.01,25.));
#17805=CARTESIAN_POINT('Origin',(-1.1,-1.01,22.9));
#17806=CARTESIAN_POINT('',(-0.726238685697896,-1.01,25.));
#17807=CARTESIAN_POINT('',(-0.726238685697896,-1.01,23.));
#17808=CARTESIAN_POINT('',(-0.726238685697896,-1.01,23.));
#17809=CARTESIAN_POINT('',(0.0305156009506911,-1.01,25.));
#17810=CARTESIAN_POINT('',(1.325,-1.01,25.));
#17811=CARTESIAN_POINT('',(0.0305156009506911,-1.01,23.));
#17812=CARTESIAN_POINT('',(0.0305156009506911,-1.01,22.9));
#17813=CARTESIAN_POINT('',(1.325,-1.01,23.));
#17814=CARTESIAN_POINT('Origin',(3.75,0.,23.));
#17815=CARTESIAN_POINT('',(1.,2.,23.));
#17816=CARTESIAN_POINT('Origin',(1.,0.,23.));
#17817=CARTESIAN_POINT('',(4.5,2.,23.));
#17818=CARTESIAN_POINT('',(6.5,2.,23.));
#17819=CARTESIAN_POINT('',(4.5,-2.,23.));
#17820=CARTESIAN_POINT('',(4.5,1.25,23.));
#17821=CARTESIAN_POINT('',(1.,-2.,23.));
#17822=CARTESIAN_POINT('',(1.,-2.,23.));
#17823=CARTESIAN_POINT('Origin',(1.,0.,23.));
#17824=CARTESIAN_POINT('Origin',(1.,0.,23.));
#17825=CARTESIAN_POINT('Origin',(1.,0.,22.9));
#17826=CARTESIAN_POINT('Origin',(1.,0.,25.));
#17827=CARTESIAN_POINT('Origin',(1.,0.,23.));
#17828=CARTESIAN_POINT('',(1.,-2.,25.));
#17829=CARTESIAN_POINT('',(1.,-2.,23.));
#17830=CARTESIAN_POINT('Origin',(1.,0.,25.));
#17831=CARTESIAN_POINT('Origin',(1.,0.,23.));
#17832=CARTESIAN_POINT('',(1.,2.,25.));
#17833=CARTESIAN_POINT('Origin',(1.,0.,25.));
#17834=CARTESIAN_POINT('',(1.,2.,23.));
#17835=CARTESIAN_POINT('Origin',(3.75,0.,25.));
#17836=CARTESIAN_POINT('',(4.5,-2.,25.));
#17837=CARTESIAN_POINT('',(1.,-2.,25.));
#17838=CARTESIAN_POINT('',(4.5,2.,25.));
#17839=CARTESIAN_POINT('',(4.5,1.25,25.));
#17840=CARTESIAN_POINT('',(6.5,2.,25.));
#17841=CARTESIAN_POINT('Origin',(1.,-2.,23.));
#17842=CARTESIAN_POINT('',(4.5,-2.,12.));
#17843=CARTESIAN_POINT('Origin',(6.5,2.,23.));
#17844=CARTESIAN_POINT('',(4.5,2.,12.));
#17845=CARTESIAN_POINT('Origin',(2.4,-1.6,14.4));
#17846=CARTESIAN_POINT('',(2.235,-1.6,14.4));
#17847=CARTESIAN_POINT('Origin',(2.4,-1.6,14.4));
#17848=CARTESIAN_POINT('',(2.235,-1.6,15.));
#17849=CARTESIAN_POINT('',(2.235,-1.6,14.4));
#17850=CARTESIAN_POINT('Origin',(2.4,-1.6,15.));
#17851=CARTESIAN_POINT('Origin',(2.4,-1.6,14.4));
#17852=CARTESIAN_POINT('Origin',(2.4,1.6,14.4));
#17853=CARTESIAN_POINT('',(2.235,1.6,14.4));
#17854=CARTESIAN_POINT('Origin',(2.4,1.6,14.4));
#17855=CARTESIAN_POINT('',(2.235,1.6,15.));
#17856=CARTESIAN_POINT('',(2.235,1.6,14.4));
#17857=CARTESIAN_POINT('Origin',(2.4,1.6,15.));
#17858=CARTESIAN_POINT('Origin',(2.4,1.6,14.4));
#17859=CARTESIAN_POINT('Origin',(0.21,1.01,12.9));
#17860=CARTESIAN_POINT('',(-0.726238685697896,1.01,13.));
#17861=CARTESIAN_POINT('',(-0.726238685697896,1.01,15.));
#17862=CARTESIAN_POINT('',(-0.726238685697896,1.01,13.));
#17863=CARTESIAN_POINT('',(0.0305156009506911,1.01,13.));
#17864=CARTESIAN_POINT('',(1.98,1.01,13.));
#17865=CARTESIAN_POINT('',(0.0305156009506911,1.01,15.));
#17866=CARTESIAN_POINT('',(0.0305156009506911,1.01,12.9));
#17867=CARTESIAN_POINT('',(1.98,1.01,15.));
#17868=CARTESIAN_POINT('Origin',(-1.1,-1.01,12.9));
#17869=CARTESIAN_POINT('',(-0.726238685697896,-1.01,15.));
#17870=CARTESIAN_POINT('',(-0.726238685697896,-1.01,13.));
#17871=CARTESIAN_POINT('',(-0.726238685697896,-1.01,13.));
#17872=CARTESIAN_POINT('',(0.0305156009506911,-1.01,15.));
#17873=CARTESIAN_POINT('',(1.325,-1.01,15.));
#17874=CARTESIAN_POINT('',(0.0305156009506911,-1.01,13.));
#17875=CARTESIAN_POINT('',(0.0305156009506911,-1.01,12.9));
#17876=CARTESIAN_POINT('',(1.325,-1.01,13.));
#17877=CARTESIAN_POINT('Origin',(3.75,0.,13.));
#17878=CARTESIAN_POINT('',(1.,2.,13.));
#17879=CARTESIAN_POINT('Origin',(1.,0.,13.));
#17880=CARTESIAN_POINT('',(4.5,2.,13.));
#17881=CARTESIAN_POINT('',(6.5,2.,13.));
#17882=CARTESIAN_POINT('',(4.5,-2.,13.));
#17883=CARTESIAN_POINT('',(4.5,1.25,13.));
#17884=CARTESIAN_POINT('',(1.,-2.,13.));
#17885=CARTESIAN_POINT('',(1.,-2.,13.));
#17886=CARTESIAN_POINT('Origin',(1.,0.,13.));
#17887=CARTESIAN_POINT('Origin',(1.,0.,13.));
#17888=CARTESIAN_POINT('Origin',(1.,0.,12.9));
#17889=CARTESIAN_POINT('Origin',(1.,0.,15.));
#17890=CARTESIAN_POINT('Origin',(1.,0.,13.));
#17891=CARTESIAN_POINT('',(1.,-2.,15.));
#17892=CARTESIAN_POINT('',(1.,-2.,13.));
#17893=CARTESIAN_POINT('Origin',(1.,0.,15.));
#17894=CARTESIAN_POINT('Origin',(1.,0.,13.));
#17895=CARTESIAN_POINT('',(1.,2.,15.));
#17896=CARTESIAN_POINT('Origin',(1.,0.,15.));
#17897=CARTESIAN_POINT('',(1.,2.,13.));
#17898=CARTESIAN_POINT('Origin',(3.75,0.,15.));
#17899=CARTESIAN_POINT('',(4.5,-2.,15.));
#17900=CARTESIAN_POINT('',(1.,-2.,15.));
#17901=CARTESIAN_POINT('',(4.5,2.,15.));
#17902=CARTESIAN_POINT('',(4.5,1.25,15.));
#17903=CARTESIAN_POINT('',(6.5,2.,15.));
#17904=CARTESIAN_POINT('Origin',(1.,-2.,13.));
#17905=CARTESIAN_POINT('',(4.5,-2.,7.));
#17906=CARTESIAN_POINT('Origin',(6.5,2.,13.));
#17907=CARTESIAN_POINT('',(4.5,2.,7.));
#17908=CARTESIAN_POINT('Origin',(7.,-3.2,0.9));
#17909=CARTESIAN_POINT('',(6.725,-3.2,1.));
#17910=CARTESIAN_POINT('Origin',(7.,-3.2,1.));
#17911=CARTESIAN_POINT('',(6.725,-3.2,2.));
#17912=CARTESIAN_POINT('',(6.725,-3.2,0.9));
#17913=CARTESIAN_POINT('Origin',(7.,-3.2,2.));
#17914=CARTESIAN_POINT('Origin',(4.,3.2,0.9));
#17915=CARTESIAN_POINT('',(3.725,3.2,1.));
#17916=CARTESIAN_POINT('Origin',(4.,3.2,1.));
#17917=CARTESIAN_POINT('',(3.725,3.2,2.));
#17918=CARTESIAN_POINT('',(3.725,3.2,0.9));
#17919=CARTESIAN_POINT('Origin',(4.,3.2,2.));
#17920=CARTESIAN_POINT('Origin',(4.,-3.2,0.9));
#17921=CARTESIAN_POINT('',(3.725,-3.2,1.));
#17922=CARTESIAN_POINT('Origin',(4.,-3.2,1.));
#17923=CARTESIAN_POINT('',(3.725,-3.2,2.));
#17924=CARTESIAN_POINT('',(3.725,-3.2,0.9));
#17925=CARTESIAN_POINT('Origin',(4.,-3.2,2.));
#17926=CARTESIAN_POINT('Origin',(7.,3.2,0.9));
#17927=CARTESIAN_POINT('',(6.725,3.2,1.));
#17928=CARTESIAN_POINT('Origin',(7.,3.2,1.));
#17929=CARTESIAN_POINT('',(6.725,3.2,2.));
#17930=CARTESIAN_POINT('',(6.725,3.2,0.9));
#17931=CARTESIAN_POINT('Origin',(7.,3.2,2.));
#17932=CARTESIAN_POINT('Origin',(5.5,0.,2.));
#17933=CARTESIAN_POINT('',(3.5,4.,2.));
#17934=CARTESIAN_POINT('',(3.5,-4.,2.));
#17935=CARTESIAN_POINT('',(3.5,4.,2.));
#17936=CARTESIAN_POINT('',(7.5,-4.,2.));
#17937=CARTESIAN_POINT('',(3.5,-4.,2.));
#17938=CARTESIAN_POINT('',(7.5,4.,2.));
#17939=CARTESIAN_POINT('',(7.5,-4.,2.));
#17940=CARTESIAN_POINT('',(7.5,4.,2.));
#17941=CARTESIAN_POINT('',(6.5,2.5,2.));
#17942=CARTESIAN_POINT('',(4.5,2.5,2.));
#17943=CARTESIAN_POINT('',(6.,2.5,2.));
#17944=CARTESIAN_POINT('',(6.5,-2.5,2.));
#17945=CARTESIAN_POINT('',(6.5,-1.25,2.));
#17946=CARTESIAN_POINT('',(4.5,-2.5,2.));
#17947=CARTESIAN_POINT('',(5.,-2.5,2.));
#17948=CARTESIAN_POINT('',(4.5,1.25,2.));
#17949=CARTESIAN_POINT('Origin',(7.5,4.,1.));
#17950=CARTESIAN_POINT('',(7.5,4.,1.));
#17951=CARTESIAN_POINT('',(3.5,4.,1.));
#17952=CARTESIAN_POINT('',(7.5,4.,1.));
#17953=CARTESIAN_POINT('',(3.5,4.,1.));
#17954=CARTESIAN_POINT('',(7.5,4.,1.));
#17955=CARTESIAN_POINT('Origin',(7.5,-4.,1.));
#17956=CARTESIAN_POINT('',(7.5,-4.,1.));
#17957=CARTESIAN_POINT('',(7.5,-4.,1.));
#17958=CARTESIAN_POINT('',(7.5,-4.,1.));
#17959=CARTESIAN_POINT('Origin',(3.5,-4.,1.));
#17960=CARTESIAN_POINT('',(3.5,-4.,1.));
#17961=CARTESIAN_POINT('',(3.5,-4.,1.));
#17962=CARTESIAN_POINT('',(3.5,-4.,1.));
#17963=CARTESIAN_POINT('Origin',(3.5,4.,1.));
#17964=CARTESIAN_POINT('',(3.5,4.,1.));
#17965=CARTESIAN_POINT('Origin',(4.5,-2.5,1.));
#17966=CARTESIAN_POINT('',(6.5,-2.5,31.));
#17967=CARTESIAN_POINT('',(6.5,-2.5,1.));
#17968=CARTESIAN_POINT('',(4.5,-2.5,31.));
#17969=CARTESIAN_POINT('',(4.5,-2.5,31.));
#17970=CARTESIAN_POINT('',(4.5,-2.5,1.));
#17971=CARTESIAN_POINT('Origin',(6.5,-2.5,1.));
#17972=CARTESIAN_POINT('',(6.5,2.5,31.));
#17973=CARTESIAN_POINT('',(6.5,2.5,1.));
#17974=CARTESIAN_POINT('',(6.5,-2.5,31.));
#17975=CARTESIAN_POINT('Origin',(6.5,2.5,1.));
#17976=CARTESIAN_POINT('',(4.5,2.5,31.));
#17977=CARTESIAN_POINT('',(4.5,2.5,1.));
#17978=CARTESIAN_POINT('',(6.5,2.5,31.));
#17979=CARTESIAN_POINT('Origin',(4.5,2.5,1.));
#17980=CARTESIAN_POINT('',(4.5,2.5,31.));
#17981=CARTESIAN_POINT('Origin',(5.5,0.,31.));
#17982=CARTESIAN_POINT('Origin',(5.5,0.,1.));
#17983=CARTESIAN_POINT('',(0.,0.,0.));
#17984=CARTESIAN_POINT('Origin',(0.21,-1.01,12.9));
#17985=CARTESIAN_POINT('',(0.21,-1.01,13.));
#17986=CARTESIAN_POINT('',(0.21,-0.621228621362538,13.));
#17987=CARTESIAN_POINT('',(0.21,-0.505,13.));
#17988=CARTESIAN_POINT('',(0.21,-1.01,15.3));
#17989=CARTESIAN_POINT('',(0.21,-1.01,12.9));
#17990=CARTESIAN_POINT('',(0.21,-0.621228621362538,15.3));
#17991=CARTESIAN_POINT('',(0.21,-0.505,15.3));
#17992=CARTESIAN_POINT('',(0.21,-0.621228621362538,13.));
#17993=CARTESIAN_POINT('Origin',(0.21,-1.01,12.9));
#17994=CARTESIAN_POINT('',(0.21,1.01,15.3));
#17995=CARTESIAN_POINT('',(0.21,0.621228621362538,15.3));
#17996=CARTESIAN_POINT('',(0.21,-0.505,15.3));
#17997=CARTESIAN_POINT('',(0.21,1.01,13.));
#17998=CARTESIAN_POINT('',(0.21,1.01,12.9));
#17999=CARTESIAN_POINT('',(0.21,0.621228621362538,13.));
#18000=CARTESIAN_POINT('',(0.21,-0.505,13.));
#18001=CARTESIAN_POINT('',(0.21,0.621228621362538,13.));
#18002=CARTESIAN_POINT('Origin',(0.21,1.01,12.9));
#18003=CARTESIAN_POINT('',(-0.240927072796786,1.01,15.3));
#18004=CARTESIAN_POINT('',(0.605,1.01,15.3));
#18005=CARTESIAN_POINT('',(-0.240927072796786,1.01,15.));
#18006=CARTESIAN_POINT('',(-0.240927072796786,1.01,15.));
#18007=CARTESIAN_POINT('',(0.0305156009506911,1.01,15.));
#18008=CARTESIAN_POINT('',(0.605,1.01,15.));
#18009=CARTESIAN_POINT('',(0.0305156009506911,1.01,13.));
#18010=CARTESIAN_POINT('',(0.0305156009506911,1.01,13.));
#18011=CARTESIAN_POINT('',(0.605,1.01,13.));
#18012=CARTESIAN_POINT('Origin',(-0.7,-1.01,12.9));
#18013=CARTESIAN_POINT('',(0.0305156009506911,-1.01,13.));
#18014=CARTESIAN_POINT('',(0.15,-1.01,13.));
#18015=CARTESIAN_POINT('',(0.0305156009506911,-1.01,15.));
#18016=CARTESIAN_POINT('',(0.0305156009506911,-1.01,13.));
#18017=CARTESIAN_POINT('',(-0.240927072796786,-1.01,15.));
#18018=CARTESIAN_POINT('',(0.15,-1.01,15.));
#18019=CARTESIAN_POINT('',(-0.240927072796786,-1.01,15.3));
#18020=CARTESIAN_POINT('',(-0.240927072796786,-1.01,15.));
#18021=CARTESIAN_POINT('',(0.15,-1.01,15.3));
#18022=CARTESIAN_POINT('Origin',(1.,0.,13.));
#18023=CARTESIAN_POINT('Origin',(1.,0.,13.));
#18024=CARTESIAN_POINT('Origin',(1.,0.,13.));
#18025=CARTESIAN_POINT('Origin',(1.,0.,13.));
#18026=CARTESIAN_POINT('Origin',(1.,0.,15.3));
#18027=CARTESIAN_POINT('Origin',(1.,0.,13.));
#18028=CARTESIAN_POINT('Origin',(1.,0.,15.));
#18029=CARTESIAN_POINT('Origin',(1.,0.,15.));
#18030=CARTESIAN_POINT('Origin',(1.,0.,15.));
#18031=CARTESIAN_POINT('Origin',(1.,0.,15.));
#18032=CARTESIAN_POINT('Origin',(1.,0.,15.3));
#18033=CARTESIAN_POINT('Origin',(1.,0.,15.3));
#18034=CARTESIAN_POINT('',(0.,0.,0.));
#18035=CARTESIAN_POINT('Origin',(2.4,-1.6,15.2));
#18036=CARTESIAN_POINT('',(2.175,-1.6,15.3));
#18037=CARTESIAN_POINT('Origin',(2.4,-1.6,15.3));
#18038=CARTESIAN_POINT('',(2.175,-1.6,15.6));
#18039=CARTESIAN_POINT('',(2.175,-1.6,15.2));
#18040=CARTESIAN_POINT('Origin',(2.4,-1.6,15.6));
#18041=CARTESIAN_POINT('Origin',(2.4,1.6,15.2));
#18042=CARTESIAN_POINT('',(2.175,1.6,15.3));
#18043=CARTESIAN_POINT('Origin',(2.4,1.6,15.3));
#18044=CARTESIAN_POINT('',(2.175,1.6,15.6));
#18045=CARTESIAN_POINT('',(2.175,1.6,15.2));
#18046=CARTESIAN_POINT('Origin',(2.4,1.6,15.6));
#18047=CARTESIAN_POINT('Origin',(0.21,1.01,15.2));
#18048=CARTESIAN_POINT('',(0.21,1.01,15.3));
#18049=CARTESIAN_POINT('',(0.,1.01,15.3));
#18050=CARTESIAN_POINT('',(0.905,1.01,15.3));
#18051=CARTESIAN_POINT('',(0.21,1.01,15.6));
#18052=CARTESIAN_POINT('',(0.21,1.01,15.2));
#18053=CARTESIAN_POINT('',(0.,1.01,15.6));
#18054=CARTESIAN_POINT('',(0.905,1.01,15.6));
#18055=CARTESIAN_POINT('',(0.,1.01,15.25));
#18056=CARTESIAN_POINT('Origin',(-0.1,-1.01,15.2));
#18057=CARTESIAN_POINT('',(0.21,-1.01,15.6));
#18058=CARTESIAN_POINT('',(0.,-1.01,15.6));
#18059=CARTESIAN_POINT('',(0.75,-1.01,15.6));
#18060=CARTESIAN_POINT('',(0.21,-1.01,15.3));
#18061=CARTESIAN_POINT('',(0.21,-1.01,15.2));
#18062=CARTESIAN_POINT('',(0.,-1.01,15.3));
#18063=CARTESIAN_POINT('',(0.75,-1.01,15.3));
#18064=CARTESIAN_POINT('',(0.,-1.01,15.25));
#18065=CARTESIAN_POINT('Origin',(0.21,-1.01,15.2));
#18066=CARTESIAN_POINT('',(0.21,-0.629285308902091,15.6));
#18067=CARTESIAN_POINT('',(0.21,-0.505,15.6));
#18068=CARTESIAN_POINT('',(0.21,-0.629285308902091,15.3));
#18069=CARTESIAN_POINT('',(0.21,-0.629285308902091,15.2));
#18070=CARTESIAN_POINT('',(0.21,-0.505,15.3));
#18071=CARTESIAN_POINT('Origin',(0.21,-1.01,15.2));
#18072=CARTESIAN_POINT('',(0.21,0.629285308902091,15.3));
#18073=CARTESIAN_POINT('',(0.21,-0.505,15.3));
#18074=CARTESIAN_POINT('',(0.21,0.629285308902091,15.6));
#18075=CARTESIAN_POINT('',(0.21,0.629285308902091,15.2));
#18076=CARTESIAN_POINT('',(0.21,-0.505,15.6));
#18077=CARTESIAN_POINT('Origin',(0.,2.2,15.3));
#18078=CARTESIAN_POINT('',(0.,2.2,15.6));
#18079=CARTESIAN_POINT('',(0.,2.2,15.6));
#18080=CARTESIAN_POINT('',(0.,2.2,15.3));
#18081=CARTESIAN_POINT('',(0.,2.2,15.3));
#18082=CARTESIAN_POINT('',(0.,2.2,15.3));
#18083=CARTESIAN_POINT('Origin',(0.,2.2,15.3));
#18084=CARTESIAN_POINT('',(0.,-2.2,15.3));
#18085=CARTESIAN_POINT('',(0.,2.2,15.3));
#18086=CARTESIAN_POINT('',(0.,-2.2,15.6));
#18087=CARTESIAN_POINT('',(0.,-2.2,15.3));
#18088=CARTESIAN_POINT('',(0.,2.2,15.6));
#18089=CARTESIAN_POINT('Origin',(1.6,0.,15.6));
#18090=CARTESIAN_POINT('Origin',(1.,0.,15.6));
#18091=CARTESIAN_POINT('',(3.2,-2.2,15.6));
#18092=CARTESIAN_POINT('',(0.,-2.2,15.6));
#18093=CARTESIAN_POINT('',(3.2,2.2,15.6));
#18094=CARTESIAN_POINT('',(3.2,-2.2,15.6));
#18095=CARTESIAN_POINT('',(3.2,2.2,15.6));
#18096=CARTESIAN_POINT('Origin',(1.,0.,15.2));
#18097=CARTESIAN_POINT('Origin',(1.,0.,15.3));
#18098=CARTESIAN_POINT('Origin',(3.2,2.2,15.3));
#18099=CARTESIAN_POINT('',(3.2,2.2,15.3));
#18100=CARTESIAN_POINT('',(3.2,2.2,15.3));
#18101=CARTESIAN_POINT('',(3.2,2.2,15.3));
#18102=CARTESIAN_POINT('Origin',(3.2,-2.2,15.3));
#18103=CARTESIAN_POINT('',(3.2,-2.2,15.3));
#18104=CARTESIAN_POINT('',(3.2,-2.2,15.3));
#18105=CARTESIAN_POINT('',(3.2,-2.2,15.3));
#18106=CARTESIAN_POINT('Origin',(0.,-2.2,15.3));
#18107=CARTESIAN_POINT('',(0.,-2.2,15.3));
#18108=CARTESIAN_POINT('Origin',(1.6,0.,15.3));
#18109=CARTESIAN_POINT('',(0.,0.,0.));
#18110=CARTESIAN_POINT('Origin',(0.21,-1.01,22.9));
#18111=CARTESIAN_POINT('',(0.21,-1.01,23.));
#18112=CARTESIAN_POINT('',(0.21,-0.621228621362538,23.));
#18113=CARTESIAN_POINT('',(0.21,-0.505,23.));
#18114=CARTESIAN_POINT('',(0.21,-1.01,25.3));
#18115=CARTESIAN_POINT('',(0.21,-1.01,22.9));
#18116=CARTESIAN_POINT('',(0.21,-0.621228621362538,25.3));
#18117=CARTESIAN_POINT('',(0.21,-0.505,25.3));
#18118=CARTESIAN_POINT('',(0.21,-0.621228621362538,23.));
#18119=CARTESIAN_POINT('Origin',(0.21,-1.01,22.9));
#18120=CARTESIAN_POINT('',(0.21,1.01,25.3));
#18121=CARTESIAN_POINT('',(0.21,0.621228621362538,25.3));
#18122=CARTESIAN_POINT('',(0.21,-0.505,25.3));
#18123=CARTESIAN_POINT('',(0.21,1.01,23.));
#18124=CARTESIAN_POINT('',(0.21,1.01,22.9));
#18125=CARTESIAN_POINT('',(0.21,0.621228621362538,23.));
#18126=CARTESIAN_POINT('',(0.21,-0.505,23.));
#18127=CARTESIAN_POINT('',(0.21,0.621228621362538,23.));
#18128=CARTESIAN_POINT('Origin',(0.21,1.01,22.9));
#18129=CARTESIAN_POINT('',(-0.240927072796786,1.01,25.3));
#18130=CARTESIAN_POINT('',(0.605,1.01,25.3));
#18131=CARTESIAN_POINT('',(-0.240927072796786,1.01,25.));
#18132=CARTESIAN_POINT('',(-0.240927072796786,1.01,25.));
#18133=CARTESIAN_POINT('',(0.0305156009506911,1.01,25.));
#18134=CARTESIAN_POINT('',(0.605,1.01,25.));
#18135=CARTESIAN_POINT('',(0.0305156009506911,1.01,23.));
#18136=CARTESIAN_POINT('',(0.0305156009506911,1.01,23.));
#18137=CARTESIAN_POINT('',(0.605,1.01,23.));
#18138=CARTESIAN_POINT('Origin',(-0.7,-1.01,22.9));
#18139=CARTESIAN_POINT('',(0.0305156009506911,-1.01,23.));
#18140=CARTESIAN_POINT('',(0.15,-1.01,23.));
#18141=CARTESIAN_POINT('',(0.0305156009506911,-1.01,25.));
#18142=CARTESIAN_POINT('',(0.0305156009506911,-1.01,23.));
#18143=CARTESIAN_POINT('',(-0.240927072796786,-1.01,25.));
#18144=CARTESIAN_POINT('',(0.15,-1.01,25.));
#18145=CARTESIAN_POINT('',(-0.240927072796786,-1.01,25.3));
#18146=CARTESIAN_POINT('',(-0.240927072796786,-1.01,25.));
#18147=CARTESIAN_POINT('',(0.15,-1.01,25.3));
#18148=CARTESIAN_POINT('Origin',(1.,0.,23.));
#18149=CARTESIAN_POINT('Origin',(1.,0.,23.));
#18150=CARTESIAN_POINT('Origin',(1.,0.,23.));
#18151=CARTESIAN_POINT('Origin',(1.,0.,23.));
#18152=CARTESIAN_POINT('Origin',(1.,0.,25.3));
#18153=CARTESIAN_POINT('Origin',(1.,0.,23.));
#18154=CARTESIAN_POINT('Origin',(1.,0.,25.));
#18155=CARTESIAN_POINT('Origin',(1.,0.,25.));
#18156=CARTESIAN_POINT('Origin',(1.,0.,25.));
#18157=CARTESIAN_POINT('Origin',(1.,0.,25.));
#18158=CARTESIAN_POINT('Origin',(1.,0.,25.3));
#18159=CARTESIAN_POINT('Origin',(1.,0.,25.3));
#18160=CARTESIAN_POINT('',(0.,0.,0.));
#18161=CARTESIAN_POINT('Origin',(2.4,-1.6,25.2));
#18162=CARTESIAN_POINT('',(2.175,-1.6,25.3));
#18163=CARTESIAN_POINT('Origin',(2.4,-1.6,25.3));
#18164=CARTESIAN_POINT('',(2.175,-1.6,25.6));
#18165=CARTESIAN_POINT('',(2.175,-1.6,25.2));
#18166=CARTESIAN_POINT('Origin',(2.4,-1.6,25.6));
#18167=CARTESIAN_POINT('Origin',(2.4,1.6,25.2));
#18168=CARTESIAN_POINT('',(2.175,1.6,25.3));
#18169=CARTESIAN_POINT('Origin',(2.4,1.6,25.3));
#18170=CARTESIAN_POINT('',(2.175,1.6,25.6));
#18171=CARTESIAN_POINT('',(2.175,1.6,25.2));
#18172=CARTESIAN_POINT('Origin',(2.4,1.6,25.6));
#18173=CARTESIAN_POINT('Origin',(0.21,1.01,25.2));
#18174=CARTESIAN_POINT('',(0.21,1.01,25.3));
#18175=CARTESIAN_POINT('',(0.,1.01,25.3));
#18176=CARTESIAN_POINT('',(0.905,1.01,25.3));
#18177=CARTESIAN_POINT('',(0.21,1.01,25.6));
#18178=CARTESIAN_POINT('',(0.21,1.01,25.2));
#18179=CARTESIAN_POINT('',(0.,1.01,25.6));
#18180=CARTESIAN_POINT('',(0.905,1.01,25.6));
#18181=CARTESIAN_POINT('',(0.,1.01,25.25));
#18182=CARTESIAN_POINT('Origin',(-0.1,-1.01,25.2));
#18183=CARTESIAN_POINT('',(0.21,-1.01,25.6));
#18184=CARTESIAN_POINT('',(0.,-1.01,25.6));
#18185=CARTESIAN_POINT('',(0.75,-1.01,25.6));
#18186=CARTESIAN_POINT('',(0.21,-1.01,25.3));
#18187=CARTESIAN_POINT('',(0.21,-1.01,25.2));
#18188=CARTESIAN_POINT('',(0.,-1.01,25.3));
#18189=CARTESIAN_POINT('',(0.75,-1.01,25.3));
#18190=CARTESIAN_POINT('',(0.,-1.01,25.25));
#18191=CARTESIAN_POINT('Origin',(0.21,-1.01,25.2));
#18192=CARTESIAN_POINT('',(0.21,-0.629285308902091,25.6));
#18193=CARTESIAN_POINT('',(0.21,-0.505,25.6));
#18194=CARTESIAN_POINT('',(0.21,-0.629285308902091,25.3));
#18195=CARTESIAN_POINT('',(0.21,-0.629285308902091,25.2));
#18196=CARTESIAN_POINT('',(0.21,-0.505,25.3));
#18197=CARTESIAN_POINT('Origin',(0.21,-1.01,25.2));
#18198=CARTESIAN_POINT('',(0.21,0.629285308902091,25.3));
#18199=CARTESIAN_POINT('',(0.21,-0.505,25.3));
#18200=CARTESIAN_POINT('',(0.21,0.629285308902091,25.6));
#18201=CARTESIAN_POINT('',(0.21,0.629285308902091,25.2));
#18202=CARTESIAN_POINT('',(0.21,-0.505,25.6));
#18203=CARTESIAN_POINT('Origin',(0.,2.2,25.3));
#18204=CARTESIAN_POINT('',(0.,2.2,25.6));
#18205=CARTESIAN_POINT('',(0.,2.2,25.6));
#18206=CARTESIAN_POINT('',(0.,2.2,25.3));
#18207=CARTESIAN_POINT('',(0.,2.2,25.3));
#18208=CARTESIAN_POINT('',(0.,2.2,25.3));
#18209=CARTESIAN_POINT('Origin',(0.,2.2,25.3));
#18210=CARTESIAN_POINT('',(0.,-2.2,25.3));
#18211=CARTESIAN_POINT('',(0.,2.2,25.3));
#18212=CARTESIAN_POINT('',(0.,-2.2,25.6));
#18213=CARTESIAN_POINT('',(0.,-2.2,25.3));
#18214=CARTESIAN_POINT('',(0.,2.2,25.6));
#18215=CARTESIAN_POINT('Origin',(1.6,0.,25.6));
#18216=CARTESIAN_POINT('Origin',(1.,0.,25.6));
#18217=CARTESIAN_POINT('',(3.2,-2.2,25.6));
#18218=CARTESIAN_POINT('',(0.,-2.2,25.6));
#18219=CARTESIAN_POINT('',(3.2,2.2,25.6));
#18220=CARTESIAN_POINT('',(3.2,-2.2,25.6));
#18221=CARTESIAN_POINT('',(3.2,2.2,25.6));
#18222=CARTESIAN_POINT('Origin',(1.,0.,25.2));
#18223=CARTESIAN_POINT('Origin',(1.,0.,25.3));
#18224=CARTESIAN_POINT('Origin',(3.2,2.2,25.3));
#18225=CARTESIAN_POINT('',(3.2,2.2,25.3));
#18226=CARTESIAN_POINT('',(3.2,2.2,25.3));
#18227=CARTESIAN_POINT('',(3.2,2.2,25.3));
#18228=CARTESIAN_POINT('Origin',(3.2,-2.2,25.3));
#18229=CARTESIAN_POINT('',(3.2,-2.2,25.3));
#18230=CARTESIAN_POINT('',(3.2,-2.2,25.3));
#18231=CARTESIAN_POINT('',(3.2,-2.2,25.3));
#18232=CARTESIAN_POINT('Origin',(0.,-2.2,25.3));
#18233=CARTESIAN_POINT('',(0.,-2.2,25.3));
#18234=CARTESIAN_POINT('Origin',(1.6,0.,25.3));
#18235=CARTESIAN_POINT('',(0.,0.,0.));
#18236=CARTESIAN_POINT('Origin',(1.,-1.8,1.6));
#18237=CARTESIAN_POINT('',(0.6,-1.8,1.6));
#18238=CARTESIAN_POINT('Origin',(1.,-1.8,1.6));
#18239=CARTESIAN_POINT('',(0.6,-1.8,2.));
#18240=CARTESIAN_POINT('',(0.6,-1.8,1.6));
#18241=CARTESIAN_POINT('Origin',(1.,-1.8,2.));
#18242=CARTESIAN_POINT('Origin',(1.,-1.8,1.6));
#18243=CARTESIAN_POINT('',(0.775,-1.8,1.6));
#18244=CARTESIAN_POINT('Origin',(1.,-1.8,1.6));
#18245=CARTESIAN_POINT('Origin',(1.,1.8,1.6));
#18246=CARTESIAN_POINT('',(0.6,1.8,1.6));
#18247=CARTESIAN_POINT('Origin',(1.,1.8,1.6));
#18248=CARTESIAN_POINT('',(0.6,1.8,2.));
#18249=CARTESIAN_POINT('',(0.6,1.8,1.6));
#18250=CARTESIAN_POINT('Origin',(1.,1.8,2.));
#18251=CARTESIAN_POINT('Origin',(1.,1.8,1.6));
#18252=CARTESIAN_POINT('',(0.775,1.8,1.6));
#18253=CARTESIAN_POINT('Origin',(1.,1.8,1.6));
#18254=CARTESIAN_POINT('Origin',(1.,-1.8,0.9));
#18255=CARTESIAN_POINT('',(0.775,-1.8,1.));
#18256=CARTESIAN_POINT('Origin',(1.,-1.8,1.));
#18257=CARTESIAN_POINT('',(0.775,-1.8,0.9));
#18258=CARTESIAN_POINT('Origin',(1.,1.8,0.9));
#18259=CARTESIAN_POINT('',(0.775,1.8,1.));
#18260=CARTESIAN_POINT('Origin',(1.,1.8,1.));
#18261=CARTESIAN_POINT('',(0.775,1.8,0.9));
#18262=CARTESIAN_POINT('Origin',(1.,0.,1.));
#18263=CARTESIAN_POINT('',(-1.5,-3.06161699786838E-16,2.));
#18264=CARTESIAN_POINT('Origin',(1.,0.,2.));
#18265=CARTESIAN_POINT('',(-1.5,-3.06161699786838E-16,1.));
#18266=CARTESIAN_POINT('',(-1.5,-3.06161699786838E-16,1.));
#18267=CARTESIAN_POINT('Origin',(1.,0.,1.));
#18268=CARTESIAN_POINT('Origin',(1.,0.,2.));
#18269=CARTESIAN_POINT('Origin',(1.,0.,1.));
#18270=CARTESIAN_POINT('',(0.,0.,0.));
#18271=CARTESIAN_POINT('Origin',(1.,0.,0.9));
#18272=CARTESIAN_POINT('',(0.15,-2.37231954002828,1.8));
#18273=CARTESIAN_POINT('',(-0.228983319658977,-2.2,1.8));
#18274=CARTESIAN_POINT('Origin',(1.,0.,1.8));
#18275=CARTESIAN_POINT('',(0.15,-2.37231954002828,1.));
#18276=CARTESIAN_POINT('',(0.15,-2.37231954002828,0.9));
#18277=CARTESIAN_POINT('',(-0.228983319658977,-2.2,1.));
#18278=CARTESIAN_POINT('Origin',(1.,0.,1.));
#18279=CARTESIAN_POINT('',(-0.228983319658977,-2.2,0.9));
#18280=CARTESIAN_POINT('Origin',(-3.25,-3.,1.));
#18281=CARTESIAN_POINT('',(0.15,-3.8,1.));
#18282=CARTESIAN_POINT('',(0.15,-3.8,1.));
#18283=CARTESIAN_POINT('',(-6.65,-3.8,1.));
#18284=CARTESIAN_POINT('',(-6.65,-3.8,1.));
#18285=CARTESIAN_POINT('',(-6.65,-2.2,1.));
#18286=CARTESIAN_POINT('',(-6.65,-3.8,1.));
#18287=CARTESIAN_POINT('',(-6.65,-2.2,1.));
#18288=CARTESIAN_POINT('',(-0.675,-3.,1.));
#18289=CARTESIAN_POINT('Origin',(-0.45,-3.,1.));
#18290=CARTESIAN_POINT('',(-6.275,-3.,1.));
#18291=CARTESIAN_POINT('Origin',(-6.05,-3.,1.));
#18292=CARTESIAN_POINT('Origin',(0.15,-3.8,1.8));
#18293=CARTESIAN_POINT('',(0.15,-3.8,1.8));
#18294=CARTESIAN_POINT('',(0.15,-3.8,1.8));
#18295=CARTESIAN_POINT('',(0.15,-3.8,1.));
#18296=CARTESIAN_POINT('Origin',(-4.66421356237309,-3.9,18.5857864376269));
#18297=CARTESIAN_POINT('',(-4.82921356237309,-3.8,18.5857864376269));
#18298=CARTESIAN_POINT('Origin',(-4.66421356237309,-3.8,18.5857864376269));
#18299=CARTESIAN_POINT('',(-4.82921356237309,-2.2,18.5857864376269));
#18300=CARTESIAN_POINT('',(-4.82921356237309,-3.9,18.5857864376269));
#18301=CARTESIAN_POINT('Origin',(-4.66421356237309,-2.2,18.5857864376269));
#18302=CARTESIAN_POINT('Origin',(-4.66421356237309,-3.9,21.4142135623731));
#18303=CARTESIAN_POINT('',(-4.82921356237309,-3.8,21.4142135623731));
#18304=CARTESIAN_POINT('Origin',(-4.66421356237309,-3.8,21.4142135623731));
#18305=CARTESIAN_POINT('',(-4.82921356237309,-2.2,21.4142135623731));
#18306=CARTESIAN_POINT('',(-4.82921356237309,-3.9,21.4142135623731));
#18307=CARTESIAN_POINT('Origin',(-4.66421356237309,-2.2,21.4142135623731));
#18308=CARTESIAN_POINT('Origin',(-1.8357864376269,-3.9,21.4142135623731));
#18309=CARTESIAN_POINT('',(-2.00078643762691,-3.8,21.4142135623731));
#18310=CARTESIAN_POINT('Origin',(-1.8357864376269,-3.8,21.4142135623731));
#18311=CARTESIAN_POINT('',(-2.00078643762691,-2.2,21.4142135623731));
#18312=CARTESIAN_POINT('',(-2.00078643762691,-3.9,21.4142135623731));
#18313=CARTESIAN_POINT('Origin',(-1.8357864376269,-2.2,21.4142135623731));
#18314=CARTESIAN_POINT('Origin',(-1.83578643762691,-3.9,18.5857864376269));
#18315=CARTESIAN_POINT('',(-2.00078643762691,-3.8,18.5857864376269));
#18316=CARTESIAN_POINT('Origin',(-1.83578643762691,-3.8,18.5857864376269));
#18317=CARTESIAN_POINT('',(-2.00078643762691,-2.2,18.5857864376269));
#18318=CARTESIAN_POINT('',(-2.00078643762691,-3.9,18.5857864376269));
#18319=CARTESIAN_POINT('Origin',(-1.83578643762691,-2.2,18.5857864376269));
#18320=CARTESIAN_POINT('Origin',(-6.05,-3.,0.9));
#18321=CARTESIAN_POINT('',(-6.275,-3.,1.8));
#18322=CARTESIAN_POINT('',(-6.275,-3.,0.9));
#18323=CARTESIAN_POINT('Origin',(-6.05,-3.,1.8));
#18324=CARTESIAN_POINT('Origin',(-0.45,-3.,0.9));
#18325=CARTESIAN_POINT('',(-0.675,-3.,1.8));
#18326=CARTESIAN_POINT('',(-0.675,-3.,0.9));
#18327=CARTESIAN_POINT('Origin',(-0.45,-3.,1.8));
#18328=CARTESIAN_POINT('Origin',(-3.25,-3.9,20.));
#18329=CARTESIAN_POINT('',(-4.85,-3.8,20.));
#18330=CARTESIAN_POINT('Origin',(-3.25,-3.8,20.));
#18331=CARTESIAN_POINT('',(-4.85,-2.2,20.));
#18332=CARTESIAN_POINT('',(-4.85,-3.9,20.));
#18333=CARTESIAN_POINT('Origin',(-3.25,-2.2,20.));
#18334=CARTESIAN_POINT('Origin',(-6.65,-3.8,1.8));
#18335=CARTESIAN_POINT('',(-0.85,-2.2,1.8));
#18336=CARTESIAN_POINT('',(0.15,-2.2,1.8));
#18337=CARTESIAN_POINT('',(-0.85,-3.8,1.8));
#18338=CARTESIAN_POINT('',(-0.85,-3.8,1.8));
#18339=CARTESIAN_POINT('',(0.15,-3.8,1.8));
#18340=CARTESIAN_POINT('Origin',(-6.65,-3.8,1.8));
#18341=CARTESIAN_POINT('',(-5.65,-2.2,1.8));
#18342=CARTESIAN_POINT('',(-5.65,-3.8,1.8));
#18343=CARTESIAN_POINT('',(-5.65,-3.,1.8));
#18344=CARTESIAN_POINT('',(-6.65,-2.2,1.8));
#18345=CARTESIAN_POINT('',(0.15,-2.2,1.8));
#18346=CARTESIAN_POINT('',(-6.65,-3.8,1.8));
#18347=CARTESIAN_POINT('',(-6.65,-3.8,1.8));
#18348=CARTESIAN_POINT('',(0.15,-3.8,1.8));
#18349=CARTESIAN_POINT('Origin',(-6.65,-3.8,1.));
#18350=CARTESIAN_POINT('',(-6.65,-3.8,1.8));
#18351=CARTESIAN_POINT('',(-6.65,-2.2,1.8));
#18352=CARTESIAN_POINT('Origin',(-5.65,-3.8,1.));
#18353=CARTESIAN_POINT('',(-0.85,-3.8,22.5));
#18354=CARTESIAN_POINT('',(-0.85,-3.8,1.));
#18355=CARTESIAN_POINT('',(-5.65,-3.8,22.5));
#18356=CARTESIAN_POINT('',(-5.65,-3.8,22.5));
#18357=CARTESIAN_POINT('',(-5.65,-3.8,1.));
#18358=CARTESIAN_POINT('Origin',(-0.85,-3.8,1.));
#18359=CARTESIAN_POINT('',(-0.85,-2.2,22.5));
#18360=CARTESIAN_POINT('',(-0.85,-2.2,1.));
#18361=CARTESIAN_POINT('',(-0.85,-3.8,22.5));
#18362=CARTESIAN_POINT('Origin',(-0.85,-2.2,1.));
#18363=CARTESIAN_POINT('',(-5.65,-2.2,22.5));
#18364=CARTESIAN_POINT('',(-5.65,-2.2,1.));
#18365=CARTESIAN_POINT('',(-0.85,-2.2,22.5));
#18366=CARTESIAN_POINT('Origin',(-5.65,-2.2,1.));
#18367=CARTESIAN_POINT('',(-5.65,-2.2,22.5));
#18368=CARTESIAN_POINT('Origin',(-3.25,-3.,22.5));
#18369=CARTESIAN_POINT('',(0.,0.,0.));
#18370=CARTESIAN_POINT('Origin',(-3.25,-4.1,20.));
#18371=CARTESIAN_POINT('',(-4.66,-4.,20.));
#18372=CARTESIAN_POINT('Origin',(-3.25,-4.,20.));
#18373=CARTESIAN_POINT('',(-4.66,-3.5,20.));
#18374=CARTESIAN_POINT('',(-4.66,-4.1,20.));
#18375=CARTESIAN_POINT('Origin',(-3.25,-3.5,20.));
#18376=CARTESIAN_POINT('Origin',(-4.66421356237309,-4.1,18.5857864376269));
#18377=CARTESIAN_POINT('',(-4.88921356237309,-4.,18.5857864376269));
#18378=CARTESIAN_POINT('Origin',(-4.66421356237309,-4.,18.5857864376269));
#18379=CARTESIAN_POINT('',(-4.88921356237309,-3.8,18.5857864376269));
#18380=CARTESIAN_POINT('',(-4.88921356237309,-4.1,18.5857864376269));
#18381=CARTESIAN_POINT('Origin',(-4.66421356237309,-3.8,18.5857864376269));
#18382=CARTESIAN_POINT('Origin',(-4.66421356237309,-4.1,21.4142135623731));
#18383=CARTESIAN_POINT('',(-4.88921356237309,-4.,21.4142135623731));
#18384=CARTESIAN_POINT('Origin',(-4.66421356237309,-4.,21.4142135623731));
#18385=CARTESIAN_POINT('',(-4.88921356237309,-3.8,21.4142135623731));
#18386=CARTESIAN_POINT('',(-4.88921356237309,-4.1,21.4142135623731));
#18387=CARTESIAN_POINT('Origin',(-4.66421356237309,-3.8,21.4142135623731));
#18388=CARTESIAN_POINT('Origin',(-1.8357864376269,-4.1,21.4142135623731));
#18389=CARTESIAN_POINT('',(-2.0607864376269,-4.,21.4142135623731));
#18390=CARTESIAN_POINT('Origin',(-1.8357864376269,-4.,21.4142135623731));
#18391=CARTESIAN_POINT('',(-2.0607864376269,-3.8,21.4142135623731));
#18392=CARTESIAN_POINT('',(-2.0607864376269,-4.1,21.4142135623731));
#18393=CARTESIAN_POINT('Origin',(-1.8357864376269,-3.8,21.4142135623731));
#18394=CARTESIAN_POINT('Origin',(-1.83578643762691,-4.1,18.5857864376269));
#18395=CARTESIAN_POINT('',(-2.06078643762691,-4.,18.5857864376269));
#18396=CARTESIAN_POINT('Origin',(-1.83578643762691,-4.,18.5857864376269));
#18397=CARTESIAN_POINT('',(-2.06078643762691,-3.8,18.5857864376269));
#18398=CARTESIAN_POINT('',(-2.06078643762691,-4.1,18.5857864376269));
#18399=CARTESIAN_POINT('Origin',(-1.83578643762691,-3.8,18.5857864376269));
#18400=CARTESIAN_POINT('Origin',(-3.25,-3.8,20.));
#18401=CARTESIAN_POINT('',(-4.84,-3.5,20.));
#18402=CARTESIAN_POINT('Origin',(-3.25,-3.5,20.));
#18403=CARTESIAN_POINT('',(-4.84,-3.8,20.));
#18404=CARTESIAN_POINT('',(-4.84,-3.8,20.));
#18405=CARTESIAN_POINT('Origin',(-3.25,-3.8,20.));
#18406=CARTESIAN_POINT('Origin',(-3.25,-3.5,20.));
#18407=CARTESIAN_POINT('Origin',(-3.25,-4.,20.));
#18408=CARTESIAN_POINT('',(-5.65,-3.8,20.));
#18409=CARTESIAN_POINT('Origin',(-3.25,-3.8,20.));
#18410=CARTESIAN_POINT('',(-5.65,-4.,20.));
#18411=CARTESIAN_POINT('',(-5.65,-4.,20.));
#18412=CARTESIAN_POINT('Origin',(-3.25,-4.,20.));
#18413=CARTESIAN_POINT('Origin',(-3.25,-3.8,20.));
#18414=CARTESIAN_POINT('Origin',(-3.25,-4.,20.));
#18415=CARTESIAN_POINT('',(0.,0.,0.));
#18416=CARTESIAN_POINT('Origin',(-3.25,-4.1,20.));
#18417=CARTESIAN_POINT('',(-4.66,-2.5,20.));
#18418=CARTESIAN_POINT('Origin',(-3.25,-2.5,20.));
#18419=CARTESIAN_POINT('',(-4.66,-2.,20.));
#18420=CARTESIAN_POINT('',(-4.66,-4.1,20.));
#18421=CARTESIAN_POINT('Origin',(-3.25,-2.,20.));
#18422=CARTESIAN_POINT('Origin',(-4.66421356237309,-2.3,18.5857864376269));
#18423=CARTESIAN_POINT('',(-4.88921356237309,-2.2,18.5857864376269));
#18424=CARTESIAN_POINT('Origin',(-4.66421356237309,-2.2,18.5857864376269));
#18425=CARTESIAN_POINT('',(-4.88921356237309,-2.,18.5857864376269));
#18426=CARTESIAN_POINT('',(-4.88921356237309,-2.3,18.5857864376269));
#18427=CARTESIAN_POINT('Origin',(-4.66421356237309,-2.,18.5857864376269));
#18428=CARTESIAN_POINT('Origin',(-4.66421356237309,-2.3,21.4142135623731));
#18429=CARTESIAN_POINT('',(-4.88921356237309,-2.2,21.4142135623731));
#18430=CARTESIAN_POINT('Origin',(-4.66421356237309,-2.2,21.4142135623731));
#18431=CARTESIAN_POINT('',(-4.88921356237309,-2.,21.4142135623731));
#18432=CARTESIAN_POINT('',(-4.88921356237309,-2.3,21.4142135623731));
#18433=CARTESIAN_POINT('Origin',(-4.66421356237309,-2.,21.4142135623731));
#18434=CARTESIAN_POINT('Origin',(-1.8357864376269,-2.3,21.4142135623731));
#18435=CARTESIAN_POINT('',(-2.0607864376269,-2.2,21.4142135623731));
#18436=CARTESIAN_POINT('Origin',(-1.8357864376269,-2.2,21.4142135623731));
#18437=CARTESIAN_POINT('',(-2.0607864376269,-2.,21.4142135623731));
#18438=CARTESIAN_POINT('',(-2.0607864376269,-2.3,21.4142135623731));
#18439=CARTESIAN_POINT('Origin',(-1.8357864376269,-2.,21.4142135623731));
#18440=CARTESIAN_POINT('Origin',(-1.83578643762691,-2.3,18.5857864376269));
#18441=CARTESIAN_POINT('',(-2.06078643762691,-2.2,18.5857864376269));
#18442=CARTESIAN_POINT('Origin',(-1.83578643762691,-2.2,18.5857864376269));
#18443=CARTESIAN_POINT('',(-2.06078643762691,-2.,18.5857864376269));
#18444=CARTESIAN_POINT('',(-2.06078643762691,-2.3,18.5857864376269));
#18445=CARTESIAN_POINT('Origin',(-1.83578643762691,-2.,18.5857864376269));
#18446=CARTESIAN_POINT('Origin',(-3.25,-2.5,20.));
#18447=CARTESIAN_POINT('',(-4.84,-2.2,20.));
#18448=CARTESIAN_POINT('Origin',(-3.25,-2.2,20.));
#18449=CARTESIAN_POINT('',(-4.84,-2.5,20.));
#18450=CARTESIAN_POINT('',(-4.84,-2.5,20.));
#18451=CARTESIAN_POINT('Origin',(-3.25,-2.5,20.));
#18452=CARTESIAN_POINT('Origin',(-3.25,-2.5,20.));
#18453=CARTESIAN_POINT('Origin',(-3.25,-2.2,20.));
#18454=CARTESIAN_POINT('',(-5.65,-2.,20.));
#18455=CARTESIAN_POINT('Origin',(-3.25,-2.,20.));
#18456=CARTESIAN_POINT('',(-5.65,-2.2,20.));
#18457=CARTESIAN_POINT('',(-5.65,-2.2,20.));
#18458=CARTESIAN_POINT('Origin',(-3.25,-2.2,20.));
#18459=CARTESIAN_POINT('Origin',(-3.25,-2.,20.));
#18460=CARTESIAN_POINT('Origin',(-3.25,-2.2,20.));
#18461=CARTESIAN_POINT('',(0.,0.,0.));
#18462=CARTESIAN_POINT('Origin',(1.,0.,0.9));
#18463=CARTESIAN_POINT('',(-0.228983319658977,2.2,1.8));
#18464=CARTESIAN_POINT('',(0.15,2.37231954002828,1.8));
#18465=CARTESIAN_POINT('Origin',(1.,0.,1.8));
#18466=CARTESIAN_POINT('',(-0.228983319658977,2.2,1.));
#18467=CARTESIAN_POINT('',(-0.228983319658977,2.2,0.9));
#18468=CARTESIAN_POINT('',(0.15,2.37231954002828,1.));
#18469=CARTESIAN_POINT('Origin',(1.,0.,1.));
#18470=CARTESIAN_POINT('',(0.15,2.37231954002828,0.9));
#18471=CARTESIAN_POINT('Origin',(-3.25,3.,1.));
#18472=CARTESIAN_POINT('',(-6.65,2.2,1.));
#18473=CARTESIAN_POINT('',(-6.65,2.2,1.));
#18474=CARTESIAN_POINT('',(-6.65,3.8,1.));
#18475=CARTESIAN_POINT('',(-6.65,2.2,1.));
#18476=CARTESIAN_POINT('',(0.15,3.8,1.));
#18477=CARTESIAN_POINT('',(-6.65,3.8,1.));
#18478=CARTESIAN_POINT('',(0.15,2.2,1.));
#18479=CARTESIAN_POINT('',(-0.675,3.,1.));
#18480=CARTESIAN_POINT('Origin',(-0.45,3.,1.));
#18481=CARTESIAN_POINT('',(-6.275,3.,1.));
#18482=CARTESIAN_POINT('Origin',(-6.05,3.,1.));
#18483=CARTESIAN_POINT('Origin',(-5.65,2.2,1.));
#18484=CARTESIAN_POINT('',(-0.85,2.2,1.8));
#18485=CARTESIAN_POINT('',(0.15,2.2,1.8));
#18486=CARTESIAN_POINT('',(-0.85,2.2,22.5));
#18487=CARTESIAN_POINT('',(-0.85,2.2,1.));
#18488=CARTESIAN_POINT('',(-5.65,2.2,22.5));
#18489=CARTESIAN_POINT('',(-5.65,2.2,22.5));
#18490=CARTESIAN_POINT('',(-5.65,2.2,1.8));
#18491=CARTESIAN_POINT('',(-5.65,2.2,1.));
#18492=CARTESIAN_POINT('',(-6.65,2.2,1.8));
#18493=CARTESIAN_POINT('',(0.15,2.2,1.8));
#18494=CARTESIAN_POINT('',(-6.65,2.2,1.8));
#18495=CARTESIAN_POINT('',(-4.82921356237309,2.2,18.5857864376269));
#18496=CARTESIAN_POINT('Origin',(-4.66421356237309,2.2,18.5857864376269));
#18497=CARTESIAN_POINT('',(-4.82921356237309,2.2,21.4142135623731));
#18498=CARTESIAN_POINT('Origin',(-4.66421356237309,2.2,21.4142135623731));
#18499=CARTESIAN_POINT('',(-2.00078643762691,2.2,21.4142135623731));
#18500=CARTESIAN_POINT('Origin',(-1.8357864376269,2.2,21.4142135623731));
#18501=CARTESIAN_POINT('',(-2.00078643762691,2.2,18.5857864376269));
#18502=CARTESIAN_POINT('Origin',(-1.83578643762691,2.2,18.5857864376269));
#18503=CARTESIAN_POINT('',(-4.85,2.2,20.));
#18504=CARTESIAN_POINT('Origin',(-3.25,2.2,20.));
#18505=CARTESIAN_POINT('Origin',(-4.66421356237309,2.1,18.5857864376269));
#18506=CARTESIAN_POINT('',(-4.82921356237309,3.8,18.5857864376269));
#18507=CARTESIAN_POINT('',(-4.82921356237309,2.1,18.5857864376269));
#18508=CARTESIAN_POINT('Origin',(-4.66421356237309,3.8,18.5857864376269));
#18509=CARTESIAN_POINT('Origin',(-4.66421356237309,2.1,21.4142135623731));
#18510=CARTESIAN_POINT('',(-4.82921356237309,3.8,21.4142135623731));
#18511=CARTESIAN_POINT('',(-4.82921356237309,2.1,21.4142135623731));
#18512=CARTESIAN_POINT('Origin',(-4.66421356237309,3.8,21.4142135623731));
#18513=CARTESIAN_POINT('Origin',(-1.8357864376269,2.1,21.4142135623731));
#18514=CARTESIAN_POINT('',(-2.00078643762691,3.8,21.4142135623731));
#18515=CARTESIAN_POINT('',(-2.00078643762691,2.1,21.4142135623731));
#18516=CARTESIAN_POINT('Origin',(-1.8357864376269,3.8,21.4142135623731));
#18517=CARTESIAN_POINT('Origin',(-1.83578643762691,2.1,18.5857864376269));
#18518=CARTESIAN_POINT('',(-2.00078643762691,3.8,18.5857864376269));
#18519=CARTESIAN_POINT('',(-2.00078643762691,2.1,18.5857864376269));
#18520=CARTESIAN_POINT('Origin',(-1.83578643762691,3.8,18.5857864376269));
#18521=CARTESIAN_POINT('Origin',(-6.05,3.,0.9));
#18522=CARTESIAN_POINT('',(-6.275,3.,1.8));
#18523=CARTESIAN_POINT('',(-6.275,3.,0.9));
#18524=CARTESIAN_POINT('Origin',(-6.05,3.,1.8));
#18525=CARTESIAN_POINT('Origin',(-0.45,3.,0.9));
#18526=CARTESIAN_POINT('',(-0.675,3.,1.8));
#18527=CARTESIAN_POINT('',(-0.675,3.,0.9));
#18528=CARTESIAN_POINT('Origin',(-0.45,3.,1.8));
#18529=CARTESIAN_POINT('Origin',(-3.25,2.1,20.));
#18530=CARTESIAN_POINT('',(-4.85,3.8,20.));
#18531=CARTESIAN_POINT('',(-4.85,2.1,20.));
#18532=CARTESIAN_POINT('Origin',(-3.25,3.8,20.));
#18533=CARTESIAN_POINT('Origin',(-6.65,2.2,1.8));
#18534=CARTESIAN_POINT('',(0.15,3.8,1.8));
#18535=CARTESIAN_POINT('',(0.15,2.2,1.8));
#18536=CARTESIAN_POINT('',(-0.85,3.8,1.8));
#18537=CARTESIAN_POINT('',(0.15,3.8,1.8));
#18538=CARTESIAN_POINT('',(-0.85,2.2,1.8));
#18539=CARTESIAN_POINT('Origin',(-6.65,2.2,1.8));
#18540=CARTESIAN_POINT('',(-5.65,3.8,1.8));
#18541=CARTESIAN_POINT('',(-5.65,3.,1.8));
#18542=CARTESIAN_POINT('',(-6.65,3.8,1.8));
#18543=CARTESIAN_POINT('',(0.15,3.8,1.8));
#18544=CARTESIAN_POINT('',(-6.65,2.2,1.8));
#18545=CARTESIAN_POINT('Origin',(-6.65,2.2,1.));
#18546=CARTESIAN_POINT('',(-6.65,3.8,1.8));
#18547=CARTESIAN_POINT('Origin',(0.15,2.2,1.8));
#18548=CARTESIAN_POINT('',(0.15,3.8,1.));
#18549=CARTESIAN_POINT('Origin',(-0.85,2.2,1.));
#18550=CARTESIAN_POINT('',(-0.85,3.8,22.5));
#18551=CARTESIAN_POINT('',(-0.85,3.8,1.));
#18552=CARTESIAN_POINT('',(-0.85,2.2,22.5));
#18553=CARTESIAN_POINT('Origin',(-0.85,3.8,1.));
#18554=CARTESIAN_POINT('',(-5.65,3.8,22.5));
#18555=CARTESIAN_POINT('',(-5.65,3.8,1.));
#18556=CARTESIAN_POINT('',(-0.85,3.8,22.5));
#18557=CARTESIAN_POINT('Origin',(-5.65,3.8,1.));
#18558=CARTESIAN_POINT('',(-5.65,3.8,22.5));
#18559=CARTESIAN_POINT('Origin',(-3.25,3.,22.5));
#18560=CARTESIAN_POINT('',(0.,0.,0.));
#18561=CARTESIAN_POINT('Origin',(-3.25,-4.1,20.));
#18562=CARTESIAN_POINT('',(-4.66,2.,20.));
#18563=CARTESIAN_POINT('Origin',(-3.25,2.,20.));
#18564=CARTESIAN_POINT('',(-4.66,2.5,20.));
#18565=CARTESIAN_POINT('',(-4.66,-4.1,20.));
#18566=CARTESIAN_POINT('Origin',(-3.25,2.5,20.));
#18567=CARTESIAN_POINT('Origin',(-4.66421356237309,1.9,18.5857864376269));
#18568=CARTESIAN_POINT('',(-4.88921356237309,2.,18.5857864376269));
#18569=CARTESIAN_POINT('Origin',(-4.66421356237309,2.,18.5857864376269));
#18570=CARTESIAN_POINT('',(-4.88921356237309,2.2,18.5857864376269));
#18571=CARTESIAN_POINT('',(-4.88921356237309,1.9,18.5857864376269));
#18572=CARTESIAN_POINT('Origin',(-4.66421356237309,2.2,18.5857864376269));
#18573=CARTESIAN_POINT('Origin',(-4.66421356237309,1.9,21.4142135623731));
#18574=CARTESIAN_POINT('',(-4.88921356237309,2.,21.4142135623731));
#18575=CARTESIAN_POINT('Origin',(-4.66421356237309,2.,21.4142135623731));
#18576=CARTESIAN_POINT('',(-4.88921356237309,2.2,21.4142135623731));
#18577=CARTESIAN_POINT('',(-4.88921356237309,1.9,21.4142135623731));
#18578=CARTESIAN_POINT('Origin',(-4.66421356237309,2.2,21.4142135623731));
#18579=CARTESIAN_POINT('Origin',(-1.8357864376269,1.9,21.4142135623731));
#18580=CARTESIAN_POINT('',(-2.0607864376269,2.,21.4142135623731));
#18581=CARTESIAN_POINT('Origin',(-1.8357864376269,2.,21.4142135623731));
#18582=CARTESIAN_POINT('',(-2.0607864376269,2.2,21.4142135623731));
#18583=CARTESIAN_POINT('',(-2.0607864376269,1.9,21.4142135623731));
#18584=CARTESIAN_POINT('Origin',(-1.8357864376269,2.2,21.4142135623731));
#18585=CARTESIAN_POINT('Origin',(-1.83578643762691,1.9,18.5857864376269));
#18586=CARTESIAN_POINT('',(-2.06078643762691,2.,18.5857864376269));
#18587=CARTESIAN_POINT('Origin',(-1.83578643762691,2.,18.5857864376269));
#18588=CARTESIAN_POINT('',(-2.06078643762691,2.2,18.5857864376269));
#18589=CARTESIAN_POINT('',(-2.06078643762691,1.9,18.5857864376269));
#18590=CARTESIAN_POINT('Origin',(-1.83578643762691,2.2,18.5857864376269));
#18591=CARTESIAN_POINT('Origin',(-3.25,2.2,20.));
#18592=CARTESIAN_POINT('',(-4.84,2.5,20.));
#18593=CARTESIAN_POINT('Origin',(-3.25,2.5,20.));
#18594=CARTESIAN_POINT('',(-4.84,2.2,20.));
#18595=CARTESIAN_POINT('',(-4.84,2.2,20.));
#18596=CARTESIAN_POINT('Origin',(-3.25,2.2,20.));
#18597=CARTESIAN_POINT('Origin',(-3.25,2.5,20.));
#18598=CARTESIAN_POINT('Origin',(-3.25,2.,20.));
#18599=CARTESIAN_POINT('',(-5.65,2.2,20.));
#18600=CARTESIAN_POINT('Origin',(-3.25,2.2,20.));
#18601=CARTESIAN_POINT('',(-5.65,2.,20.));
#18602=CARTESIAN_POINT('',(-5.65,2.,20.));
#18603=CARTESIAN_POINT('Origin',(-3.25,2.,20.));
#18604=CARTESIAN_POINT('Origin',(-3.25,2.2,20.));
#18605=CARTESIAN_POINT('Origin',(-3.25,2.,20.));
#18606=CARTESIAN_POINT('',(0.,0.,0.));
#18607=CARTESIAN_POINT('Origin',(-3.25,-4.1,20.));
#18608=CARTESIAN_POINT('',(-4.66,3.5,20.));
#18609=CARTESIAN_POINT('Origin',(-3.25,3.5,20.));
#18610=CARTESIAN_POINT('',(-4.66,4.,20.));
#18611=CARTESIAN_POINT('',(-4.66,-4.1,20.));
#18612=CARTESIAN_POINT('Origin',(-3.25,4.,20.));
#18613=CARTESIAN_POINT('Origin',(-4.66421356237309,3.7,18.5857864376269));
#18614=CARTESIAN_POINT('',(-4.88921356237309,3.8,18.5857864376269));
#18615=CARTESIAN_POINT('Origin',(-4.66421356237309,3.8,18.5857864376269));
#18616=CARTESIAN_POINT('',(-4.88921356237309,4.,18.5857864376269));
#18617=CARTESIAN_POINT('',(-4.88921356237309,3.7,18.5857864376269));
#18618=CARTESIAN_POINT('Origin',(-4.66421356237309,4.,18.5857864376269));
#18619=CARTESIAN_POINT('Origin',(-4.66421356237309,3.7,21.4142135623731));
#18620=CARTESIAN_POINT('',(-4.88921356237309,3.8,21.4142135623731));
#18621=CARTESIAN_POINT('Origin',(-4.66421356237309,3.8,21.4142135623731));
#18622=CARTESIAN_POINT('',(-4.88921356237309,4.,21.4142135623731));
#18623=CARTESIAN_POINT('',(-4.88921356237309,3.7,21.4142135623731));
#18624=CARTESIAN_POINT('Origin',(-4.66421356237309,4.,21.4142135623731));
#18625=CARTESIAN_POINT('Origin',(-1.8357864376269,3.7,21.4142135623731));
#18626=CARTESIAN_POINT('',(-2.0607864376269,3.8,21.4142135623731));
#18627=CARTESIAN_POINT('Origin',(-1.8357864376269,3.8,21.4142135623731));
#18628=CARTESIAN_POINT('',(-2.0607864376269,4.,21.4142135623731));
#18629=CARTESIAN_POINT('',(-2.0607864376269,3.7,21.4142135623731));
#18630=CARTESIAN_POINT('Origin',(-1.8357864376269,4.,21.4142135623731));
#18631=CARTESIAN_POINT('Origin',(-1.83578643762691,3.7,18.5857864376269));
#18632=CARTESIAN_POINT('',(-2.06078643762691,3.8,18.5857864376269));
#18633=CARTESIAN_POINT('Origin',(-1.83578643762691,3.8,18.5857864376269));
#18634=CARTESIAN_POINT('',(-2.06078643762691,4.,18.5857864376269));
#18635=CARTESIAN_POINT('',(-2.06078643762691,3.7,18.5857864376269));
#18636=CARTESIAN_POINT('Origin',(-1.83578643762691,4.,18.5857864376269));
#18637=CARTESIAN_POINT('Origin',(-3.25,3.5,20.));
#18638=CARTESIAN_POINT('',(-4.84,3.8,20.));
#18639=CARTESIAN_POINT('Origin',(-3.25,3.8,20.));
#18640=CARTESIAN_POINT('',(-4.84,3.5,20.));
#18641=CARTESIAN_POINT('',(-4.84,3.5,20.));
#18642=CARTESIAN_POINT('Origin',(-3.25,3.5,20.));
#18643=CARTESIAN_POINT('Origin',(-3.25,3.5,20.));
#18644=CARTESIAN_POINT('Origin',(-3.25,3.8,20.));
#18645=CARTESIAN_POINT('',(-5.65,4.,20.));
#18646=CARTESIAN_POINT('Origin',(-3.25,4.,20.));
#18647=CARTESIAN_POINT('',(-5.65,3.8,20.));
#18648=CARTESIAN_POINT('',(-5.65,3.8,20.));
#18649=CARTESIAN_POINT('Origin',(-3.25,3.8,20.));
#18650=CARTESIAN_POINT('Origin',(-3.25,4.,20.));
#18651=CARTESIAN_POINT('Origin',(-3.25,3.8,20.));
#18652=CARTESIAN_POINT('',(0.,0.,0.));
#18653=CARTESIAN_POINT('Origin',(0.375,0.5,0.));
#18654=CARTESIAN_POINT('',(-0.375,0.5,-4.59242549680257E-17));
#18655=CARTESIAN_POINT('Origin',(0.,0.5,0.));
#18656=CARTESIAN_POINT('Origin',(0.,0.475,0.));
#18657=CARTESIAN_POINT('',(-0.425,0.45,-5.20474889637625E-17));
#18658=CARTESIAN_POINT('Origin',(0.,0.45,0.));
#18659=CARTESIAN_POINT('',(-0.4,0.475,-4.89858719658941E-17));
#18660=CARTESIAN_POINT('Origin',(0.,0.24,0.));
#18661=CARTESIAN_POINT('',(-0.425,0.0299999999999998,-5.20474889637625E-17));
#18662=CARTESIAN_POINT('Origin',(0.,0.0299999999999998,0.));
#18663=CARTESIAN_POINT('',(-0.425,0.24,-5.20474889637625E-17));
#18664=CARTESIAN_POINT('Origin',(0.,0.0150000000000001,0.));
#18665=CARTESIAN_POINT('',(-0.395,4.85722573273506E-17,-4.83735485663204E-17));
#18666=CARTESIAN_POINT('Origin',(0.,0.,0.));
#18667=CARTESIAN_POINT('',(-0.41,0.0150000000000001,-5.02105187650415E-17));
#18668=CARTESIAN_POINT('Origin',(0.27,0.,0.));
#18669=CARTESIAN_POINT('',(-0.27,0.,-3.30654635769785E-17));
#18670=CARTESIAN_POINT('Origin',(0.,0.,0.));
#18671=CARTESIAN_POINT('Origin',(0.,-0.02,0.));
#18672=CARTESIAN_POINT('',(-0.24505,-0.0498999999999999,3.00099698131059E-17));
#18673=CARTESIAN_POINT('Origin',(0.,-0.0498999999999999,0.));
#18674=CARTESIAN_POINT('',(-0.26,-0.02,-3.18408167778312E-17));
#18675=CARTESIAN_POINT('Origin',(0.,-0.995,0.));
#18676=CARTESIAN_POINT('',(-0.24505,-1.95495,3.00099698131059E-17));
#18677=CARTESIAN_POINT('Origin',(0.,-1.95495,0.));
#18678=CARTESIAN_POINT('',(-0.24505,-0.995,-3.00099698131059E-17));
#18679=CARTESIAN_POINT('Origin',(0.,-1.975,0.));
#18680=CARTESIAN_POINT('',(-0.2,-2.,-2.44929359829471E-17));
#18681=CARTESIAN_POINT('Origin',(0.,-2.,0.));
#18682=CARTESIAN_POINT('',(-0.225,-1.975,-2.75545529808154E-17));
#18683=CARTESIAN_POINT('Origin',(0.,-2.,0.));
#18684=CARTESIAN_POINT('Origin',(0.115470053837925,-0.5,-0.2));
#18685=CARTESIAN_POINT('',(0.23094010767585,-0.5,0.));
#18686=CARTESIAN_POINT('',(0.115470053837925,-0.5,-0.2));
#18687=CARTESIAN_POINT('',(0.23094010767585,-0.5,0.));
#18688=CARTESIAN_POINT('',(0.115470053837925,-0.8,-0.2));
#18689=CARTESIAN_POINT('',(0.115470053837925,-0.5,-0.2));
#18690=CARTESIAN_POINT('',(0.23094010767585,-0.8,0.));
#18691=CARTESIAN_POINT('',(0.23094010767585,-0.8,0.));
#18692=CARTESIAN_POINT('',(0.23094010767585,-0.5,0.));
#18693=CARTESIAN_POINT('Origin',(-0.115470053837925,-0.5,-0.2));
#18694=CARTESIAN_POINT('',(-0.115470053837925,-0.5,-0.2));
#18695=CARTESIAN_POINT('',(0.115470053837925,-0.5,-0.2));
#18696=CARTESIAN_POINT('',(-0.115470053837925,-0.8,-0.2));
#18697=CARTESIAN_POINT('',(-0.115470053837925,-0.5,-0.2));
#18698=CARTESIAN_POINT('',(0.115470053837925,-0.8,-0.2));
#18699=CARTESIAN_POINT('Origin',(-0.23094010767585,-0.5,-2.77555756156289E-17));
#18700=CARTESIAN_POINT('',(-0.23094010767585,-0.5,-2.82820063659975E-17));
#18701=CARTESIAN_POINT('',(-0.115470053837925,-0.5,-0.2));
#18702=CARTESIAN_POINT('',(-0.23094010767585,-0.8,-2.77555756156289E-17));
#18703=CARTESIAN_POINT('',(-0.23094010767585,-0.5,-2.82820063659975E-17));
#18704=CARTESIAN_POINT('',(-0.115470053837925,-0.8,-0.2));
#18705=CARTESIAN_POINT('Origin',(-0.115470053837925,-0.5,0.2));
#18706=CARTESIAN_POINT('',(-0.115470053837925,-0.5,0.2));
#18707=CARTESIAN_POINT('',(-0.23094010767585,-0.5,-2.82820063659975E-17));
#18708=CARTESIAN_POINT('',(-0.115470053837925,-0.8,0.2));
#18709=CARTESIAN_POINT('',(-0.115470053837925,-0.5,0.2));
#18710=CARTESIAN_POINT('',(-0.23094010767585,-0.8,-2.82820063659975E-17));
#18711=CARTESIAN_POINT('Origin',(0.115470053837925,-0.5,0.2));
#18712=CARTESIAN_POINT('',(0.115470053837925,-0.5,0.2));
#18713=CARTESIAN_POINT('',(-0.115470053837925,-0.5,0.2));
#18714=CARTESIAN_POINT('',(0.115470053837925,-0.8,0.2));
#18715=CARTESIAN_POINT('',(0.115470053837925,-0.5,0.2));
#18716=CARTESIAN_POINT('',(-0.115470053837925,-0.8,0.2));
#18717=CARTESIAN_POINT('Origin',(0.23094010767585,-0.5,0.));
#18718=CARTESIAN_POINT('',(0.115470053837925,-0.5,0.2));
#18719=CARTESIAN_POINT('',(0.115470053837925,-0.8,0.2));
#18720=CARTESIAN_POINT('Origin',(0.,-0.5,0.));
#18721=CARTESIAN_POINT('Origin',(0.,-0.8,0.));
#18722=CARTESIAN_POINT('',(0.,0.,0.));
#18723=CARTESIAN_POINT('',(0.,0.,0.));
#18724=CARTESIAN_POINT('Origin',(0.,0.,0.));
#18725=CARTESIAN_POINT('',(-1.070235,-0.308121667383195,-1.31065986708547E-16));
#18726=CARTESIAN_POINT('',(-1.31065986708547E-16,-0.308121667383195,1.070235));
#18727=CARTESIAN_POINT('Origin',(0.,-0.308121667383195,0.));
#18728=CARTESIAN_POINT('Origin',(0.,-0.308121667383195,0.));
#18729=CARTESIAN_POINT('',(-1.31065986708547E-16,0.308121667383195,1.070235));
#18730=CARTESIAN_POINT('Origin',(-1.34711147906209E-16,0.,1.1));
#18731=CARTESIAN_POINT('',(-1.070235,0.308121667383195,1.31065986708547E-16));
#18732=CARTESIAN_POINT('Origin',(0.,0.308121667383195,0.));
#18733=CARTESIAN_POINT('Origin',(0.,0.308121667383195,0.));
#18734=CARTESIAN_POINT('Origin',(0.,0.,0.));
#18735=CARTESIAN_POINT('',(-1.070235,0.5,-1.31065986708547E-16));
#18736=CARTESIAN_POINT('',(-1.070235,0.,-1.31065986708547E-16));
#18737=CARTESIAN_POINT('Origin',(0.,0.5,0.));
#18738=CARTESIAN_POINT('Origin',(0.,0.,0.));
#18739=CARTESIAN_POINT('',(-0.6,-0.44,-7.34788079488412E-17));
#18740=CARTESIAN_POINT('Origin',(0.,-0.44,0.));
#18741=CARTESIAN_POINT('',(-0.6,0.44,-7.34788079488412E-17));
#18742=CARTESIAN_POINT('',(-0.6,0.,-7.34788079488412E-17));
#18743=CARTESIAN_POINT('Origin',(0.,0.44,0.));
#18744=CARTESIAN_POINT('Origin',(0.,0.47,0.));
#18745=CARTESIAN_POINT('',(-0.66,0.5,-8.08266887437253E-17));
#18746=CARTESIAN_POINT('',(-0.63,0.47,-7.71527483462832E-17));
#18747=CARTESIAN_POINT('Origin',(0.,0.5,0.));
#18748=CARTESIAN_POINT('Origin',(1.070235,0.5,0.));
#18749=CARTESIAN_POINT('Origin',(0.,0.,0.));
#18750=CARTESIAN_POINT('',(-1.070235,-0.5,-1.31065986708547E-16));
#18751=CARTESIAN_POINT('Origin',(0.,-0.5,0.));
#18752=CARTESIAN_POINT('',(-1.070235,0.,-1.31065986708547E-16));
#18753=CARTESIAN_POINT('Origin',(0.66,-0.5,0.));
#18754=CARTESIAN_POINT('',(-0.66,-0.5,-8.08266887437253E-17));
#18755=CARTESIAN_POINT('Origin',(0.,-0.5,0.));
#18756=CARTESIAN_POINT('Origin',(0.,-0.47,0.));
#18757=CARTESIAN_POINT('',(-0.63,-0.47,-7.71527483462832E-17));
#18758=CARTESIAN_POINT('',(0.,0.,0.));
#18759=CARTESIAN_POINT('Origin',(0.,0.,0.));
#18760=CARTESIAN_POINT('',(-1.129765,0.308121667383195,-1.38356309103871E-16));
#18761=CARTESIAN_POINT('',(-1.38356309103871E-16,0.308121667383195,1.129765));
#18762=CARTESIAN_POINT('Origin',(0.,0.308121667383195,0.));
#18763=CARTESIAN_POINT('Origin',(0.,0.308121667383195,0.));
#18764=CARTESIAN_POINT('',(-1.38356309103871E-16,-0.308121667383195,1.129765));
#18765=CARTESIAN_POINT('Origin',(-1.34711147906209E-16,0.,1.1));
#18766=CARTESIAN_POINT('',(-1.129765,-0.308121667383195,1.38356309103871E-16));
#18767=CARTESIAN_POINT('Origin',(0.,-0.308121667383195,0.));
#18768=CARTESIAN_POINT('Origin',(0.,-0.308121667383195,0.));
#18769=CARTESIAN_POINT('Origin',(0.,0.,0.));
#18770=CARTESIAN_POINT('',(-1.129765,-0.5,-1.38356309103871E-16));
#18771=CARTESIAN_POINT('Origin',(0.,-0.5,0.));
#18772=CARTESIAN_POINT('',(-1.129765,0.,-1.38356309103871E-16));
#18773=CARTESIAN_POINT('Origin',(1.54,0.5,0.));
#18774=CARTESIAN_POINT('',(-1.54,0.5,-1.88595607068692E-16));
#18775=CARTESIAN_POINT('Origin',(0.,0.5,0.));
#18776=CARTESIAN_POINT('',(-1.129765,0.5,-1.38356309103871E-16));
#18777=CARTESIAN_POINT('Origin',(0.,0.5,0.));
#18778=CARTESIAN_POINT('Origin',(0.,0.47,0.));
#18779=CARTESIAN_POINT('',(-1.6,0.44,-1.95943487863577E-16));
#18780=CARTESIAN_POINT('Origin',(0.,0.44,0.));
#18781=CARTESIAN_POINT('',(-1.57,0.47,-1.92269547466134E-16));
#18782=CARTESIAN_POINT('Origin',(0.,0.,0.));
#18783=CARTESIAN_POINT('',(-1.6,-0.44,-1.95943487863577E-16));
#18784=CARTESIAN_POINT('Origin',(0.,-0.44,0.));
#18785=CARTESIAN_POINT('',(-1.6,0.,-1.95943487863577E-16));
#18786=CARTESIAN_POINT('Origin',(0.,-0.47,0.));
#18787=CARTESIAN_POINT('',(-1.54,-0.5,-1.88595607068692E-16));
#18788=CARTESIAN_POINT('Origin',(0.,-0.5,0.));
#18789=CARTESIAN_POINT('',(-1.57,-0.47,-1.92269547466134E-16));
#18790=CARTESIAN_POINT('Origin',(1.129765,-0.5,0.));
#18791=CARTESIAN_POINT('Origin',(0.,0.,0.));
#18792=CARTESIAN_POINT('',(-1.129765,0.,-1.38356309103871E-16));
#18793=CARTESIAN_POINT('',(0.,0.,0.));
#18794=CARTESIAN_POINT('Origin',(1.1,0.,0.));
#18795=CARTESIAN_POINT('',(1.1,-2.23201749654651E-33,0.29765));
#18796=CARTESIAN_POINT('',(1.1,-2.23201749654651E-33,-0.29765));
#18797=CARTESIAN_POINT('Origin',(1.1,0.,0.));
#18798=CARTESIAN_POINT('Origin',(0.685838782044607,0.,-0.860014630714833));
#18799=CARTESIAN_POINT('',(0.918550922801216,-5.31350540756609E-33,-0.674432891191581));
#18800=CARTESIAN_POINT('',(0.453126641287998,8.49470414473068E-34,-1.04559637023808));
#18801=CARTESIAN_POINT('Origin',(0.685838782044607,0.,-0.860014630714833));
#18802=CARTESIAN_POINT('Origin',(-0.244773027351946,0.,-1.07242070340001));
#18803=CARTESIAN_POINT('',(0.0454142657089739,-2.23201749654651E-33,-1.1386540593921));
#18804=CARTESIAN_POINT('',(-0.534960320412865,-2.23201749654651E-33,-1.00618734740791));
#18805=CARTESIAN_POINT('Origin',(-0.244773027351946,0.,-1.07242070340001));
#18806=CARTESIAN_POINT('Origin',(-0.991065754692661,0.,-0.477272113029314));
#18807=CARTESIAN_POINT('',(-0.86192025974432,8.49470414473067E-34,-0.745445496560469));
#18808=CARTESIAN_POINT('',(-1.120211249641,-5.31350540756609E-33,-0.209098729498159));
#18809=CARTESIAN_POINT('Origin',(-0.991065754692661,0.,-0.477272113029314));
#18810=CARTESIAN_POINT('Origin',(-0.991065754692661,0.,0.477272113029314));
#18811=CARTESIAN_POINT('',(-1.120211249641,-2.23201749654651E-33,0.209098729498159));
#18812=CARTESIAN_POINT('',(-0.86192025974432,-2.23201749654651E-33,0.745445496560469));
#18813=CARTESIAN_POINT('Origin',(-0.991065754692661,0.,0.477272113029314));
#18814=CARTESIAN_POINT('Origin',(-0.244773027351946,0.,1.07242070340001));
#18815=CARTESIAN_POINT('',(-0.534960320412866,-2.23201749654651E-33,1.00618734740791));
#18816=CARTESIAN_POINT('',(0.0454142657089737,-2.23201749654651E-33,1.1386540593921));
#18817=CARTESIAN_POINT('Origin',(-0.244773027351946,0.,1.07242070340001));
#18818=CARTESIAN_POINT('Origin',(0.685838782044607,0.,0.860014630714833));
#18819=CARTESIAN_POINT('',(0.453126641287998,-2.23201749654651E-33,1.04559637023808));
#18820=CARTESIAN_POINT('',(0.918550922801216,-2.23201749654651E-33,0.674432891191581));
#18821=CARTESIAN_POINT('Origin',(0.685838782044607,0.,0.860014630714833));
#18822=CARTESIAN_POINT('',(0.,0.,0.));
#18823=CARTESIAN_POINT('Origin',(0.685838782044607,0.,0.860014630714833));
#18824=CARTESIAN_POINT('',(0.413083465285518,-0.05953,0.993751811093549));
#18825=CARTESIAN_POINT('',(0.876916659919095,-0.05953,0.623857181492959));
#18826=CARTESIAN_POINT('Ctrl Pts',(0.413083465285518,-0.05953,0.993751811093549));
#18827=CARTESIAN_POINT('Ctrl Pts',(0.419070565453383,-0.0925528133349865,
0.991263089003441));
#18828=CARTESIAN_POINT('Ctrl Pts',(0.430199341854858,-0.124911173756694,
0.986608710139579));
#18829=CARTESIAN_POINT('Ctrl Pts',(0.457978755888596,-0.177924977804098,
0.973971221090534));
#18830=CARTESIAN_POINT('Ctrl Pts',(0.473077587363685,-0.199697230012983,
0.966820759530997));
#18831=CARTESIAN_POINT('Ctrl Pts',(0.507057380724533,-0.237895043532788,
0.949440676105255));
#18832=CARTESIAN_POINT('Ctrl Pts',(0.525933334162555,-0.254319232363049,
0.939198248544428));
#18833=CARTESIAN_POINT('Ctrl Pts',(0.564362943424238,-0.28018331644634,
0.916597376014514));
#18834=CARTESIAN_POINT('Ctrl Pts',(0.585840553788742,-0.29104845371857,
0.903141581680914));
#18835=CARTESIAN_POINT('Ctrl Pts',(0.629305439856167,-0.30527573347708,
0.873412008702649));
#18836=CARTESIAN_POINT('Ctrl Pts',(0.651278921914856,-0.308638795020976,
0.857118508332695));
#18837=CARTESIAN_POINT('Ctrl Pts',(0.690705563850638,-0.308638795020976,
0.825676810575914));
#18838=CARTESIAN_POINT('Ctrl Pts',(0.711480111898423,-0.30527573347708,
0.807879894508811));
#18839=CARTESIAN_POINT('Ctrl Pts',(0.750136149454208,-0.29104845371857,
0.772120216227122));
#18840=CARTESIAN_POINT('Ctrl Pts',(0.768033796848072,-0.28018331644634,
0.754175290318038));
#18841=CARTESIAN_POINT('Ctrl Pts',(0.798619410861634,-0.254319232363049,
0.721738358858166));
#18842=CARTESIAN_POINT('Ctrl Pts',(0.812805334167529,-0.237895043532788,
0.705614819529209));
#18843=CARTESIAN_POINT('Ctrl Pts',(0.837310877969633,-0.199697230012983,
0.676354402927683));
#18844=CARTESIAN_POINT('Ctrl Pts',(0.847641868610495,-0.177924977804098,
0.663225258065736));
#18845=CARTESIAN_POINT('Ctrl Pts',(0.866144010579847,-0.124911173756694,
0.638954437806245));
#18846=CARTESIAN_POINT('Ctrl Pts',(0.873158080166742,-0.0925528133349865,
0.62914037979579));
#18847=CARTESIAN_POINT('Ctrl Pts',(0.876916659919095,-0.05953,0.623857181492959));
#18848=CARTESIAN_POINT('',(0.437601487681057,-0.05953,1.03511272300331));
#18849=CARTESIAN_POINT('Origin',(0.685838782044607,-0.05953,0.860014630714833));
#18850=CARTESIAN_POINT('',(0.911784794170997,-0.05953,0.656964154625313));
#18851=CARTESIAN_POINT('Ctrl Pts',(0.911784794170998,-0.0595300000000001,
0.656964154625312));
#18852=CARTESIAN_POINT('Ctrl Pts',(0.909827729890942,-0.0762225747374255,
0.659680317203144));
#18853=CARTESIAN_POINT('Ctrl Pts',(0.907004864562642,-0.0928409665394228,
0.663576540841106));
#18854=CARTESIAN_POINT('Ctrl Pts',(0.895234408667242,-0.144299303100741,
0.679480524217551));
#18855=CARTESIAN_POINT('Ctrl Pts',(0.882797231409153,-0.177024326825049,
0.695831250979106));
#18856=CARTESIAN_POINT('Ctrl Pts',(0.854332839576145,-0.227269801620064,
0.73042219438957));
#18857=CARTESIAN_POINT('Ctrl Pts',(0.834863020612702,-0.251265615809407,
0.752807465209441));
#18858=CARTESIAN_POINT('Ctrl Pts',(0.800439809856111,-0.279889827963178,
0.789147407129766));
#18859=CARTESIAN_POINT('Ctrl Pts',(0.781998747691871,-0.290879136862659,
0.80756613568454));
#18860=CARTESIAN_POINT('Ctrl Pts',(0.742239891936898,-0.305251990234487,
0.844254137480382));
#18861=CARTESIAN_POINT('Ctrl Pts',(0.720906778729541,-0.308638795020976,
0.862505527716294));
#18862=CARTESIAN_POINT('Ctrl Pts',(0.680463863683392,-0.308638795020976,
0.894757676234429));
#18863=CARTESIAN_POINT('Ctrl Pts',(0.657923009631182,-0.305251990234488,
0.91149460735272));
#18864=CARTESIAN_POINT('Ctrl Pts',(0.613307674922609,-0.290879136862659,
0.942092777160053));
#18865=CARTESIAN_POINT('Ctrl Pts',(0.591247219971725,-0.279889827963178,
0.955972930713954));
#18866=CARTESIAN_POINT('Ctrl Pts',(0.548158511259202,-0.251265615809407,
0.981446681891443));
#18867=CARTESIAN_POINT('Ctrl Pts',(0.522002043615455,-0.227269801620063,
0.995447160474328));
#18868=CARTESIAN_POINT('Ctrl Pts',(0.481944444320713,-0.177024326825049,
1.01550068154148));
#18869=CARTESIAN_POINT('Ctrl Pts',(0.463236132117164,-0.14429930310074,
1.0239876538093));
#18870=CARTESIAN_POINT('Ctrl Pts',(0.445111721969657,-0.0928409665394226,
1.03192403056628));
#18871=CARTESIAN_POINT('Ctrl Pts',(0.440685038163619,-0.0762225747374254,
1.03380912944435));
#18872=CARTESIAN_POINT('Ctrl Pts',(0.437601487681056,-0.05953,1.03511272300331));
#18873=CARTESIAN_POINT('Origin',(0.685838782044607,-0.05953,0.860014630714833));
#18874=CARTESIAN_POINT('Origin',(0.,-0.208355,0.));
#18875=CARTESIAN_POINT('',(0.0548532617164168,-0.05953,1.12247250791415));
#18876=CARTESIAN_POINT('Origin',(0.,-0.05953,0.));
#18877=CARTESIAN_POINT('',(-0.536443649899848,-0.05953,0.987512846410683));
#18878=CARTESIAN_POINT('Ctrl Pts',(0.0548532617164173,-0.0595300000000001,
1.12247250791414));
#18879=CARTESIAN_POINT('Ctrl Pts',(0.05150947068137,-0.0762225747374254,
1.12263591311425));
#18880=CARTESIAN_POINT('Ctrl Pts',(0.0467032526342597,-0.0928409665394227,
1.12285816383385));
#18881=CARTESIAN_POINT('Ctrl Pts',(0.0269302585198975,-0.144299303100741,
1.12357162229597));
#18882=CARTESIAN_POINT('Ctrl Pts',(0.006392292392153,-0.177024326825049,
1.12404235695137));
#18883=CARTESIAN_POINT('Ctrl Pts',(-0.0383992541984087,-0.227269801620063,
1.12335509974011));
#18884=CARTESIAN_POINT('Ctrl Pts',(-0.0680399972366993,-0.251265615809407,
1.12208997038458));
#18885=CARTESIAN_POINT('Ctrl Pts',(-0.117914228755037,-0.279889827963178,
1.1178344036749));
#18886=CARTESIAN_POINT('Ctrl Pts',(-0.14381238480104,-0.290879136862659,
1.11490049012186));
#18887=CARTESIAN_POINT('Ctrl Pts',(-0.19728546073067,-0.305251990234488,
1.10669035995599));
#18888=CARTESIAN_POINT('Ctrl Pts',(-0.224855950742601,-0.308638795020976,
1.10139101611326));
#18889=CARTESIAN_POINT('Ctrl Pts',(-0.275287440920027,-0.308638795020976,
1.0898803575765));
#18890=CARTESIAN_POINT('Ctrl Pts',(-0.302426893214945,-0.305251990234488,
1.08269251410343));
#18891=CARTESIAN_POINT('Ctrl Pts',(-0.35416671187353,-0.290879136862659,
1.06688848765783));
#18892=CARTESIAN_POINT('Ctrl Pts',(-0.3787731215897,-0.279889827963178,
1.05829506364875));
#18893=CARTESIAN_POINT('Ctrl Pts',(-0.425554672694338,-0.251265615809407,
1.04048957871266));
#18894=CARTESIAN_POINT('Ctrl Pts',(-0.452808978448581,-0.227269801620063,
1.02876878445619));
#18895=CARTESIAN_POINT('Ctrl Pts',(-0.493462957200432,-0.177024326825049,
1.0099536580922));
#18896=CARTESIAN_POINT('Ctrl Pts',(-0.511762781179148,-0.14429930310074,
1.00061845128527));
#18897=CARTESIAN_POINT('Ctrl Pts',(-0.529268075276157,-0.0928409665394226,
0.991396466802468));
#18898=CARTESIAN_POINT('Ctrl Pts',(-0.533501897135713,-0.0762225747374254,
0.989110885965947));
#18899=CARTESIAN_POINT('Ctrl Pts',(-0.536443649899848,-0.0595300000000001,
0.987512846410683));
#18900=CARTESIAN_POINT('',(-0.843383895613249,-0.05953,0.742736168477219));
#18901=CARTESIAN_POINT('Origin',(0.,-0.05953,0.));
#18902=CARTESIAN_POINT('',(-1.10653577764992,-0.05953,0.196295654879792));
#18903=CARTESIAN_POINT('Ctrl Pts',(-0.843383895613249,-0.0595300000000001,
0.742736168477219));
#18904=CARTESIAN_POINT('Ctrl Pts',(-0.84559647055299,-0.0762225747374255,
0.740223768851062));
#18905=CARTESIAN_POINT('Ctrl Pts',(-0.848766861100456,-0.0928409665394227,
0.736604687327351));
#18906=CARTESIAN_POINT('Ctrl Pts',(-0.861652925570091,-0.144299303100741,
0.721590372101268));
#18907=CARTESIAN_POINT('Ctrl Pts',(-0.87482617317514,-0.177024326825049,
0.705826641853758));
#18908=CARTESIAN_POINT('Ctrl Pts',(-0.902215926359523,-0.227269801620063,
0.670378702718353));
#18909=CARTESIAN_POINT('Ctrl Pts',(-0.919707509403859,-0.251265615809407,
0.646415841396062));
#18910=CARTESIAN_POINT('Ctrl Pts',(-0.947476448101718,-0.279889827963178,
0.604769294586516));
#18911=CARTESIAN_POINT('Ctrl Pts',(-0.961329858300736,-0.290879136862659,
0.582692035672022));
#18912=CARTESIAN_POINT('Ctrl Pts',(-0.988250837578047,-0.305251990234488,
0.535766169015486));
#18913=CARTESIAN_POINT('Ctrl Pts',(-1.00129756308006,-0.308638795020976,
0.510906605094603));
#18914=CARTESIAN_POINT('Ctrl Pts',(-1.02374168767024,-0.308638795020976,
0.46430090015576));
#18915=CARTESIAN_POINT('Ctrl Pts',(-1.03504317708586,-0.305251990234488,
0.438600874831839));
#18916=CARTESIAN_POINT('Ctrl Pts',(-1.05494634094458,-0.290879136862659,
0.388295406390235));
#18917=CARTESIAN_POINT('Ctrl Pts',(-1.06356957703048,-0.279889827963178,
0.363699428370917));
#18918=CARTESIAN_POINT('Ctrl Pts',(-1.0788165083757,-0.251265615809407,
0.316022600643821));
#18919=CARTESIAN_POINT('Ctrl Pts',(-1.08664560412098,-0.227269801620063,
0.287406530683752));
#18920=CARTESIAN_POINT('Ctrl Pts',(-1.09728268713976,-0.177024326825049,
0.243890930799337));
#18921=CARTESIAN_POINT('Ctrl Pts',(-1.10139388218929,-0.144299303100741,
0.22376314604679));
#18922=CARTESIAN_POINT('Ctrl Pts',(-1.10509821673782,-0.0928409665394227,
0.204327142733961));
#18923=CARTESIAN_POINT('Ctrl Pts',(-1.10595102243643,-0.0762225747374254,
0.199591971170104));
#18924=CARTESIAN_POINT('Ctrl Pts',(-1.10653577764992,-0.0595300000000001,
0.196295654879792));
#18925=CARTESIAN_POINT('',(-1.123812,-0.05953,1.37627276864339E-16));
#18926=CARTESIAN_POINT('Origin',(0.,-0.05953,0.));
#18927=CARTESIAN_POINT('',(-1.123812,-0.35718,1.37627276864339E-16));
#18928=CARTESIAN_POINT('',(-1.123812,-0.208355,1.37627276864339E-16));
#18929=CARTESIAN_POINT('Origin',(0.,-0.35718,0.));
#18930=CARTESIAN_POINT('',(-1.10653577764992,-0.05953,-0.196295654879793));
#18931=CARTESIAN_POINT('Origin',(0.,-0.05953,0.));
#18932=CARTESIAN_POINT('',(-0.843383895613249,-0.05953,-0.742736168477219));
#18933=CARTESIAN_POINT('Ctrl Pts',(-1.10653577764992,-0.0595300000000001,
-0.196295654879792));
#18934=CARTESIAN_POINT('Ctrl Pts',(-1.10595102243643,-0.0762225747374255,
-0.199591971170104));
#18935=CARTESIAN_POINT('Ctrl Pts',(-1.10509821673782,-0.0928409665394228,
-0.204327142733962));
#18936=CARTESIAN_POINT('Ctrl Pts',(-1.10139388218929,-0.144299303100741,
-0.22376314604679));
#18937=CARTESIAN_POINT('Ctrl Pts',(-1.09728268713976,-0.177024326825049,
-0.243890930799338));
#18938=CARTESIAN_POINT('Ctrl Pts',(-1.08664560412098,-0.227269801620063,
-0.287406530683753));
#18939=CARTESIAN_POINT('Ctrl Pts',(-1.0788165083757,-0.251265615809407,
-0.316022600643821));
#18940=CARTESIAN_POINT('Ctrl Pts',(-1.06356957703048,-0.279889827963178,
-0.363699428370918));
#18941=CARTESIAN_POINT('Ctrl Pts',(-1.05494634094458,-0.290879136862659,
-0.388295406390235));
#18942=CARTESIAN_POINT('Ctrl Pts',(-1.03504317708586,-0.305251990234488,
-0.438600874831839));
#18943=CARTESIAN_POINT('Ctrl Pts',(-1.02374168767024,-0.308638795020976,
-0.46430090015576));
#18944=CARTESIAN_POINT('Ctrl Pts',(-1.00129756308006,-0.308638795020976,
-0.510906605094603));
#18945=CARTESIAN_POINT('Ctrl Pts',(-0.988250837578047,-0.305251990234488,
-0.535766169015486));
#18946=CARTESIAN_POINT('Ctrl Pts',(-0.961329858300736,-0.290879136862659,
-0.582692035672022));
#18947=CARTESIAN_POINT('Ctrl Pts',(-0.947476448101718,-0.279889827963178,
-0.604769294586516));
#18948=CARTESIAN_POINT('Ctrl Pts',(-0.919707509403859,-0.251265615809407,
-0.646415841396062));
#18949=CARTESIAN_POINT('Ctrl Pts',(-0.902215926359523,-0.227269801620064,
-0.670378702718353));
#18950=CARTESIAN_POINT('Ctrl Pts',(-0.87482617317514,-0.177024326825049,
-0.705826641853758));
#18951=CARTESIAN_POINT('Ctrl Pts',(-0.861652925570091,-0.144299303100741,
-0.721590372101268));
#18952=CARTESIAN_POINT('Ctrl Pts',(-0.848766861100456,-0.0928409665394229,
-0.736604687327351));
#18953=CARTESIAN_POINT('Ctrl Pts',(-0.84559647055299,-0.0762225747374255,
-0.740223768851063));
#18954=CARTESIAN_POINT('Ctrl Pts',(-0.843383895613249,-0.0595300000000001,
-0.742736168477219));
#18955=CARTESIAN_POINT('',(-0.536443649899847,-0.05953,-0.987512846410683));
#18956=CARTESIAN_POINT('Origin',(0.,-0.05953,0.));
#18957=CARTESIAN_POINT('',(0.0548532617164172,-0.05953,-1.12247250791415));
#18958=CARTESIAN_POINT('Ctrl Pts',(-0.536443649899848,-0.0595300000000001,
-0.987512846410683));
#18959=CARTESIAN_POINT('Ctrl Pts',(-0.533501897135712,-0.0762225747374254,
-0.989110885965947));
#18960=CARTESIAN_POINT('Ctrl Pts',(-0.529268075276156,-0.0928409665394227,
-0.991396466802469));
#18961=CARTESIAN_POINT('Ctrl Pts',(-0.511762781179147,-0.144299303100741,
-1.00061845128527));
#18962=CARTESIAN_POINT('Ctrl Pts',(-0.493462957200432,-0.177024326825049,
-1.0099536580922));
#18963=CARTESIAN_POINT('Ctrl Pts',(-0.45280897844858,-0.227269801620063,
-1.02876878445619));
#18964=CARTESIAN_POINT('Ctrl Pts',(-0.425554672694337,-0.251265615809407,
-1.04048957871266));
#18965=CARTESIAN_POINT('Ctrl Pts',(-0.3787731215897,-0.279889827963178,
-1.05829506364875));
#18966=CARTESIAN_POINT('Ctrl Pts',(-0.354166711873529,-0.290879136862659,
-1.06688848765783));
#18967=CARTESIAN_POINT('Ctrl Pts',(-0.302426893214944,-0.305251990234488,
-1.08269251410343));
#18968=CARTESIAN_POINT('Ctrl Pts',(-0.275287440920027,-0.308638795020976,
-1.0898803575765));
#18969=CARTESIAN_POINT('Ctrl Pts',(-0.224855950742601,-0.308638795020976,
-1.10139101611326));
#18970=CARTESIAN_POINT('Ctrl Pts',(-0.19728546073067,-0.305251990234488,
-1.10669035995599));
#18971=CARTESIAN_POINT('Ctrl Pts',(-0.143812384801039,-0.290879136862659,
-1.11490049012186));
#18972=CARTESIAN_POINT('Ctrl Pts',(-0.117914228755037,-0.279889827963178,
-1.1178344036749));
#18973=CARTESIAN_POINT('Ctrl Pts',(-0.0680399972366989,-0.251265615809407,
-1.12208997038458));
#18974=CARTESIAN_POINT('Ctrl Pts',(-0.0383992541984084,-0.227269801620063,
-1.12335509974011));
#18975=CARTESIAN_POINT('Ctrl Pts',(0.00639229239215326,-0.177024326825049,
-1.12404235695137));
#18976=CARTESIAN_POINT('Ctrl Pts',(0.0269302585198977,-0.144299303100741,
-1.12357162229597));
#18977=CARTESIAN_POINT('Ctrl Pts',(0.04670325263426,-0.0928409665394228,
-1.12285816383385));
#18978=CARTESIAN_POINT('Ctrl Pts',(0.0515094706813703,-0.0762225747374255,
-1.12263591311425));
#18979=CARTESIAN_POINT('Ctrl Pts',(0.0548532617164176,-0.0595300000000001,
-1.12247250791414));
#18980=CARTESIAN_POINT('',(0.437601487681057,-0.05953,-1.03511272300331));
#18981=CARTESIAN_POINT('Origin',(0.,-0.05953,0.));
#18982=CARTESIAN_POINT('',(0.911784794170997,-0.05953,-0.656964154625313));
#18983=CARTESIAN_POINT('Ctrl Pts',(0.437601487681056,-0.0595300000000001,
-1.03511272300331));
#18984=CARTESIAN_POINT('Ctrl Pts',(0.440685038163619,-0.0762225747374255,
-1.03380912944435));
#18985=CARTESIAN_POINT('Ctrl Pts',(0.445111721969657,-0.0928409665394228,
-1.03192403056628));
#18986=CARTESIAN_POINT('Ctrl Pts',(0.463236132117164,-0.144299303100741,
-1.0239876538093));
#18987=CARTESIAN_POINT('Ctrl Pts',(0.481944444320713,-0.177024326825049,
-1.01550068154148));
#18988=CARTESIAN_POINT('Ctrl Pts',(0.522002043615455,-0.227269801620064,
-0.995447160474328));
#18989=CARTESIAN_POINT('Ctrl Pts',(0.548158511259203,-0.251265615809407,
-0.981446681891443));
#18990=CARTESIAN_POINT('Ctrl Pts',(0.591247219971725,-0.279889827963178,
-0.955972930713954));
#18991=CARTESIAN_POINT('Ctrl Pts',(0.613307674922609,-0.290879136862659,
-0.942092777160053));
#18992=CARTESIAN_POINT('Ctrl Pts',(0.657923009631182,-0.305251990234487,
-0.91149460735272));
#18993=CARTESIAN_POINT('Ctrl Pts',(0.680463863683393,-0.308638795020976,
-0.894757676234429));
#18994=CARTESIAN_POINT('Ctrl Pts',(0.720906778729542,-0.308638795020976,
-0.862505527716294));
#18995=CARTESIAN_POINT('Ctrl Pts',(0.742239891936899,-0.305251990234488,
-0.844254137480381));
#18996=CARTESIAN_POINT('Ctrl Pts',(0.781998747691872,-0.290879136862659,
-0.80756613568454));
#18997=CARTESIAN_POINT('Ctrl Pts',(0.800439809856112,-0.279889827963178,
-0.789147407129765));
#18998=CARTESIAN_POINT('Ctrl Pts',(0.834863020612702,-0.251265615809407,
-0.752807465209441));
#18999=CARTESIAN_POINT('Ctrl Pts',(0.854332839576145,-0.227269801620064,
-0.73042219438957));
#19000=CARTESIAN_POINT('Ctrl Pts',(0.882797231409153,-0.177024326825049,
-0.695831250979106));
#19001=CARTESIAN_POINT('Ctrl Pts',(0.895234408667242,-0.144299303100741,
-0.679480524217551));
#19002=CARTESIAN_POINT('Ctrl Pts',(0.907004864562642,-0.0928409665394228,
-0.663576540841106));
#19003=CARTESIAN_POINT('Ctrl Pts',(0.909827729890942,-0.0762225747374256,
-0.659680317203144));
#19004=CARTESIAN_POINT('Ctrl Pts',(0.911784794170998,-0.0595300000000001,
-0.656964154625312));
#19005=CARTESIAN_POINT('',(1.08212377959455,-0.05953,-0.303251606722892));
#19006=CARTESIAN_POINT('Origin',(0.,-0.05953,0.));
#19007=CARTESIAN_POINT('',(1.08212377959455,-0.05953,0.303251606722892));
#19008=CARTESIAN_POINT('Ctrl Pts',(1.08212377959455,-0.0595300000000001,
-0.303251606722892));
#19009=CARTESIAN_POINT('Ctrl Pts',(1.0830271513892,-0.0762225747374255,
-0.300028012588062));
#19010=CARTESIAN_POINT('Ctrl Pts',(1.08431331394788,-0.0928409665394228,
-0.2953917518996));
#19011=CARTESIAN_POINT('Ctrl Pts',(1.08940878963422,-0.144299303100741,
-0.276273267473431));
#19012=CARTESIAN_POINT('Ctrl Pts',(1.09443784939331,-0.177024326825049,
-0.256354979351213));
#19013=CARTESIAN_POINT('Ctrl Pts',(1.10373487993589,-0.227269801620064,
-0.212533521233765));
#19014=CARTESIAN_POINT('Ctrl Pts',(1.10909715583869,-0.251265615809407,
-0.183354415742157));
#19015=CARTESIAN_POINT('Ctrl Pts',(1.1160463456491,-0.279889827963178,-0.133783682657561));
#19016=CARTESIAN_POINT('Ctrl Pts',(1.11894887330541,-0.290879136862659,
-0.107881990270302));
#19017=CARTESIAN_POINT('Ctrl Pts',(1.12284346704144,-0.305251990234488,
-0.0539226701638766));
#19018=CARTESIAN_POINT('Ctrl Pts',(1.123812,-0.308638795020976,-0.025864214957475));
#19019=CARTESIAN_POINT('Ctrl Pts',(1.123812,-0.308638795020976,0.025864214957475));
#19020=CARTESIAN_POINT('Ctrl Pts',(1.12284346704144,-0.305251990234488,
0.0539226701638766));
#19021=CARTESIAN_POINT('Ctrl Pts',(1.11894887330541,-0.290879136862659,
0.107881990270302));
#19022=CARTESIAN_POINT('Ctrl Pts',(1.1160463456491,-0.279889827963178,0.133783682657561));
#19023=CARTESIAN_POINT('Ctrl Pts',(1.10909715583869,-0.251265615809407,
0.183354415742157));
#19024=CARTESIAN_POINT('Ctrl Pts',(1.10373487993589,-0.227269801620064,
0.212533521233765));
#19025=CARTESIAN_POINT('Ctrl Pts',(1.09443784939331,-0.177024326825049,
0.256354979351213));
#19026=CARTESIAN_POINT('Ctrl Pts',(1.08940878963422,-0.144299303100741,
0.276273267473431));
#19027=CARTESIAN_POINT('Ctrl Pts',(1.08431331394788,-0.0928409665394228,
0.2953917518996));
#19028=CARTESIAN_POINT('Ctrl Pts',(1.0830271513892,-0.0762225747374255,
0.300028012588062));
#19029=CARTESIAN_POINT('Ctrl Pts',(1.08212377959455,-0.0595300000000001,
0.303251606722892));
#19030=CARTESIAN_POINT('Origin',(0.,-0.05953,0.));
#19031=CARTESIAN_POINT('Origin',(0.,-0.05953,0.));
#19032=CARTESIAN_POINT('',(0.0589974094846122,-0.05953,1.07456964270265));
#19033=CARTESIAN_POINT('Origin',(0.,-0.05953,0.));
#19034=CARTESIAN_POINT('Origin',(-0.244773027351946,-0.05953,1.07242070340001));
#19035=CARTESIAN_POINT('Origin',(-0.244773027351946,0.,1.07242070340001));
#19036=CARTESIAN_POINT('',(-0.519393123750572,-0.05953,0.942555777842682));
#19037=CARTESIAN_POINT('Ctrl Pts',(-0.519393123750572,-0.05953,0.942555777842682));
#19038=CARTESIAN_POINT('Ctrl Pts',(-0.513714466572041,-0.0925528133349865,
0.945684988399766));
#19039=CARTESIAN_POINT('Ctrl Pts',(-0.503136848051455,-0.124911173756694,
0.951483858396181));
#19040=CARTESIAN_POINT('Ctrl Pts',(-0.47593627990192,-0.177924977804098,
0.965323333309091));
#19041=CARTESIAN_POINT('Ctrl Pts',(-0.460931856495794,-0.199697230012983,
0.972669835243841));
#19042=CARTESIAN_POINT('Ctrl Pts',(-0.426157505475872,-0.237895043532788,
0.988400002689705));
#19043=CARTESIAN_POINT('Ctrl Pts',(-0.406380688682952,-0.254319232363049,
0.996771768218699));
#19044=CARTESIAN_POINT('Ctrl Pts',(-0.364750145543744,-0.28018331644634,
1.01272583306292));
#19045=CARTESIAN_POINT('Ctrl Pts',(-0.340838910881557,-0.29104845371857,
1.02112815447116));
#19046=CARTESIAN_POINT('Ctrl Pts',(-0.290495481564827,-0.30527573347708,
1.036574285215));
#19047=CARTESIAN_POINT('Ctrl Pts',(-0.264056468041074,-0.308638795020976,
1.04359501395068));
#19048=CARTESIAN_POINT('Ctrl Pts',(-0.214892249704082,-0.308638795020976,
1.05481642595959));
#19049=CARTESIAN_POINT('Ctrl Pts',(-0.188025341585962,-0.30527573347708,
1.05996242598502));
#19050=CARTESIAN_POINT('Ctrl Pts',(-0.135965654106109,-0.29104845371857,
1.06788913840721));
#19051=CARTESIAN_POINT('Ctrl Pts',(-0.110776745452494,-0.28018331644634,
1.07069360430242));
#19052=CARTESIAN_POINT('Ctrl Pts',(-0.0663467128214646,-0.254319232363049,
1.07438230428002));
#19053=CARTESIAN_POINT('Ctrl Pts',(-0.0448960436540983,-0.237895043532788,
1.07542044338697));
#19054=CARTESIAN_POINT('Ctrl Pts',(-0.00674037211528124,-0.199697230012983,
1.07633607767727));
#19055=CARTESIAN_POINT('Ctrl Pts',(0.00996567398334777,-0.177924977804098,
1.07622728347683));
#19056=CARTESIAN_POINT('Ctrl Pts',(0.0404772621979741,-0.124911173756694,
1.07556023164702));
#19057=CARTESIAN_POINT('Ctrl Pts',(0.0525234025782719,-0.0925528133349865,
1.07492508698591));
#19058=CARTESIAN_POINT('Ctrl Pts',(0.0589974094846124,-0.05953,1.07456964270265));
#19059=CARTESIAN_POINT('Origin',(-0.244773027351946,-0.05953,1.07242070340001));
#19060=CARTESIAN_POINT('Origin',(0.,-0.05953,0.));
#19061=CARTESIAN_POINT('',(-0.803348093619616,-0.05953,0.716109245731214));
#19062=CARTESIAN_POINT('Origin',(0.,-0.05953,0.));
#19063=CARTESIAN_POINT('Origin',(-0.991065754692661,-0.05953,0.477272113029314));
#19064=CARTESIAN_POINT('Origin',(-0.991065754692661,0.,0.477272113029314));
#19065=CARTESIAN_POINT('',(-1.06075609691358,-0.05953,0.181596019242328));
#19066=CARTESIAN_POINT('Ctrl Pts',(-1.06075609691358,-0.05953,0.181596019242328));
#19067=CARTESIAN_POINT('Ctrl Pts',(-1.05966202740332,-0.0925528133349865,
0.187986803072856));
#19068=CARTESIAN_POINT('Ctrl Pts',(-1.05760072925372,-0.124911173756694,
0.199872254546857));
#19069=CARTESIAN_POINT('Ctrl Pts',(-1.05146158959546,-0.177924977804098,
0.22976728653846));
#19070=CARTESIAN_POINT('Ctrl Pts',(-1.04785021111757,-0.199697230012983,
0.246078686169301));
#19071=CARTESIAN_POINT('Ctrl Pts',(-1.03846709802406,-0.237895043532788,
0.283073967563097));
#19072=CARTESIAN_POINT('Ctrl Pts',(-1.03268176429485,-0.254319232363049,
0.303755815985685));
#19073=CARTESIAN_POINT('Ctrl Pts',(-1.01919893537026,-0.28018331644634,
0.346251081972725));
#19074=CARTESIAN_POINT('Ctrl Pts',(-1.01085972381132,-0.29104845371857,
0.370184399726282));
#19075=CARTESIAN_POINT('Ctrl Pts',(-0.99154738033959,-0.30527573347708,
0.419174982698463));
#19076=CARTESIAN_POINT('Ctrl Pts',(-0.980551951791748,-0.308638795020976,
0.444223188605045));
#19077=CARTESIAN_POINT('Ctrl Pts',(-0.958671816228589,-0.308638795020976,
0.489657758261848));
#19078=CARTESIAN_POINT('Ctrl Pts',(-0.945943877838127,-0.30527573347708,
0.51387163140139));
#19079=CARTESIAN_POINT('Ctrl Pts',(-0.91968254693063,-0.29104845371857,
0.559515758398093));
#19080=CARTESIAN_POINT('Ctrl Pts',(-0.906170138993533,-0.28018331644634,
0.580957796077825));
#19081=CARTESIAN_POINT('Ctrl Pts',(-0.8813524085237,-0.254319232363049,
0.617994461173994));
#19082=CARTESIAN_POINT('Ctrl Pts',(-0.868789784891799,-0.237895043532788,
0.635412538795143));
#19083=CARTESIAN_POINT('Ctrl Pts',(-0.845715984518854,-0.199697230012983,
0.66581473268113));
#19084=CARTESIAN_POINT('Ctrl Pts',(-0.835214876415962,-0.177924977804098,
0.678808213394124));
#19085=CARTESIAN_POINT('Ctrl Pts',(-0.815669690204649,-0.124911173756694,
0.702247233627224));
#19086=CARTESIAN_POINT('Ctrl Pts',(-0.807662468433796,-0.0925528133349865,
0.711269279199861));
#19087=CARTESIAN_POINT('Ctrl Pts',(-0.803348093619616,-0.05953,0.716109245731214));
#19088=CARTESIAN_POINT('Origin',(-0.991065754692661,-0.05953,0.477272113029314));
#19089=CARTESIAN_POINT('Origin',(0.,-0.05953,0.));
#19090=CARTESIAN_POINT('',(-1.076188,-0.05953,1.31795018948079E-16));
#19091=CARTESIAN_POINT('Origin',(0.,-0.05953,0.));
#19092=CARTESIAN_POINT('',(-1.06075609691358,-0.05953,-0.181596019242328));
#19093=CARTESIAN_POINT('Origin',(0.,-0.05953,0.));
#19094=CARTESIAN_POINT('Origin',(-0.991065754692661,-0.05953,-0.477272113029314));
#19095=CARTESIAN_POINT('Origin',(-0.991065754692661,0.,-0.477272113029314));
#19096=CARTESIAN_POINT('',(-0.803348093619616,-0.05953,-0.716109245731215));
#19097=CARTESIAN_POINT('Ctrl Pts',(-0.803348093619616,-0.05953,-0.716109245731215));
#19098=CARTESIAN_POINT('Ctrl Pts',(-0.807662468433795,-0.0925528133349865,
-0.711269279199862));
#19099=CARTESIAN_POINT('Ctrl Pts',(-0.815669690204649,-0.124911173756694,
-0.702247233627224));
#19100=CARTESIAN_POINT('Ctrl Pts',(-0.835214876415962,-0.177924977804098,
-0.678808213394124));
#19101=CARTESIAN_POINT('Ctrl Pts',(-0.845715984518854,-0.199697230012983,
-0.66581473268113));
#19102=CARTESIAN_POINT('Ctrl Pts',(-0.868789784891799,-0.237895043532788,
-0.635412538795143));
#19103=CARTESIAN_POINT('Ctrl Pts',(-0.8813524085237,-0.254319232363049,
-0.617994461173994));
#19104=CARTESIAN_POINT('Ctrl Pts',(-0.906170138993533,-0.28018331644634,
-0.580957796077826));
#19105=CARTESIAN_POINT('Ctrl Pts',(-0.91968254693063,-0.29104845371857,
-0.559515758398093));
#19106=CARTESIAN_POINT('Ctrl Pts',(-0.945943877838127,-0.30527573347708,
-0.51387163140139));
#19107=CARTESIAN_POINT('Ctrl Pts',(-0.958671816228589,-0.308638795020976,
-0.489657758261848));
#19108=CARTESIAN_POINT('Ctrl Pts',(-0.980551951791748,-0.308638795020976,
-0.444223188605045));
#19109=CARTESIAN_POINT('Ctrl Pts',(-0.99154738033959,-0.30527573347708,
-0.419174982698463));
#19110=CARTESIAN_POINT('Ctrl Pts',(-1.01085972381132,-0.29104845371857,
-0.370184399726282));
#19111=CARTESIAN_POINT('Ctrl Pts',(-1.01919893537026,-0.28018331644634,
-0.346251081972725));
#19112=CARTESIAN_POINT('Ctrl Pts',(-1.03268176429485,-0.254319232363049,
-0.303755815985685));
#19113=CARTESIAN_POINT('Ctrl Pts',(-1.03846709802406,-0.237895043532788,
-0.283073967563097));
#19114=CARTESIAN_POINT('Ctrl Pts',(-1.04785021111757,-0.199697230012983,
-0.246078686169302));
#19115=CARTESIAN_POINT('Ctrl Pts',(-1.05146158959546,-0.177924977804098,
-0.229767286538461));
#19116=CARTESIAN_POINT('Ctrl Pts',(-1.05760072925372,-0.124911173756694,
-0.199872254546858));
#19117=CARTESIAN_POINT('Ctrl Pts',(-1.05966202740332,-0.0925528133349864,
-0.187986803072857));
#19118=CARTESIAN_POINT('Ctrl Pts',(-1.06075609691358,-0.05953,-0.181596019242328));
#19119=CARTESIAN_POINT('Origin',(-0.991065754692661,-0.05953,-0.477272113029314));
#19120=CARTESIAN_POINT('Origin',(0.,-0.05953,0.));
#19121=CARTESIAN_POINT('',(-0.519393123750572,-0.05953,-0.942555777842682));
#19122=CARTESIAN_POINT('Origin',(0.,-0.05953,0.));
#19123=CARTESIAN_POINT('Origin',(-0.244773027351946,-0.05953,-1.07242070340001));
#19124=CARTESIAN_POINT('Origin',(-0.244773027351946,0.,-1.07242070340001));
#19125=CARTESIAN_POINT('',(0.0589974094846125,-0.05953,-1.07456964270265));
#19126=CARTESIAN_POINT('Ctrl Pts',(0.0589974094846127,-0.05953,-1.07456964270265));
#19127=CARTESIAN_POINT('Ctrl Pts',(0.0525234025782722,-0.0925528133349865,
-1.07492508698591));
#19128=CARTESIAN_POINT('Ctrl Pts',(0.0404772621979744,-0.124911173756694,
-1.07556023164702));
#19129=CARTESIAN_POINT('Ctrl Pts',(0.0099656739833481,-0.177924977804098,
-1.07622728347683));
#19130=CARTESIAN_POINT('Ctrl Pts',(-0.00674037211528096,-0.199697230012983,
-1.07633607767727));
#19131=CARTESIAN_POINT('Ctrl Pts',(-0.044896043654098,-0.237895043532788,
-1.07542044338697));
#19132=CARTESIAN_POINT('Ctrl Pts',(-0.0663467128214644,-0.254319232363049,
-1.07438230428002));
#19133=CARTESIAN_POINT('Ctrl Pts',(-0.110776745452493,-0.28018331644634,
-1.07069360430242));
#19134=CARTESIAN_POINT('Ctrl Pts',(-0.135965654106109,-0.29104845371857,
-1.06788913840721));
#19135=CARTESIAN_POINT('Ctrl Pts',(-0.188025341585962,-0.30527573347708,
-1.05996242598502));
#19136=CARTESIAN_POINT('Ctrl Pts',(-0.214892249704082,-0.308638795020976,
-1.05481642595959));
#19137=CARTESIAN_POINT('Ctrl Pts',(-0.264056468041074,-0.308638795020976,
-1.04359501395068));
#19138=CARTESIAN_POINT('Ctrl Pts',(-0.290495481564827,-0.30527573347708,
-1.036574285215));
#19139=CARTESIAN_POINT('Ctrl Pts',(-0.340838910881557,-0.291048453718569,
-1.02112815447116));
#19140=CARTESIAN_POINT('Ctrl Pts',(-0.364750145543744,-0.28018331644634,
-1.01272583306292));
#19141=CARTESIAN_POINT('Ctrl Pts',(-0.406380688682952,-0.254319232363049,
-0.996771768218699));
#19142=CARTESIAN_POINT('Ctrl Pts',(-0.426157505475872,-0.237895043532788,
-0.988400002689705));
#19143=CARTESIAN_POINT('Ctrl Pts',(-0.460931856495794,-0.199697230012983,
-0.972669835243841));
#19144=CARTESIAN_POINT('Ctrl Pts',(-0.475936279901919,-0.177924977804098,
-0.965323333309091));
#19145=CARTESIAN_POINT('Ctrl Pts',(-0.503136848051454,-0.124911173756694,
-0.951483858396181));
#19146=CARTESIAN_POINT('Ctrl Pts',(-0.513714466572041,-0.0925528133349865,
-0.945684988399766));
#19147=CARTESIAN_POINT('Ctrl Pts',(-0.519393123750572,-0.05953,-0.942555777842682));
#19148=CARTESIAN_POINT('Origin',(-0.244773027351946,-0.05953,-1.07242070340001));
#19149=CARTESIAN_POINT('Origin',(0.,-0.05953,0.));
#19150=CARTESIAN_POINT('',(0.413083465285518,-0.05953,-0.993751811093549));
#19151=CARTESIAN_POINT('Origin',(0.,-0.05953,0.));
#19152=CARTESIAN_POINT('Origin',(0.685838782044607,-0.05953,-0.860014630714833));
#19153=CARTESIAN_POINT('Origin',(0.685838782044607,0.,-0.860014630714833));
#19154=CARTESIAN_POINT('',(0.876916659919095,-0.05953,-0.623857181492959));
#19155=CARTESIAN_POINT('Ctrl Pts',(0.876916659919095,-0.05953,-0.623857181492958));
#19156=CARTESIAN_POINT('Ctrl Pts',(0.873158080166742,-0.0925528133349865,
-0.62914037979579));
#19157=CARTESIAN_POINT('Ctrl Pts',(0.866144010579847,-0.124911173756694,
-0.638954437806245));
#19158=CARTESIAN_POINT('Ctrl Pts',(0.847641868610495,-0.177924977804098,
-0.663225258065736));
#19159=CARTESIAN_POINT('Ctrl Pts',(0.837310877969633,-0.199697230012983,
-0.676354402927683));
#19160=CARTESIAN_POINT('Ctrl Pts',(0.81280533416753,-0.237895043532788,
-0.705614819529209));
#19161=CARTESIAN_POINT('Ctrl Pts',(0.798619410861634,-0.254319232363049,
-0.721738358858166));
#19162=CARTESIAN_POINT('Ctrl Pts',(0.768033796848072,-0.28018331644634,
-0.754175290318038));
#19163=CARTESIAN_POINT('Ctrl Pts',(0.750136149454208,-0.29104845371857,
-0.772120216227122));
#19164=CARTESIAN_POINT('Ctrl Pts',(0.711480111898423,-0.30527573347708,
-0.807879894508811));
#19165=CARTESIAN_POINT('Ctrl Pts',(0.690705563850638,-0.308638795020976,
-0.825676810575913));
#19166=CARTESIAN_POINT('Ctrl Pts',(0.651278921914856,-0.308638795020976,
-0.857118508332695));
#19167=CARTESIAN_POINT('Ctrl Pts',(0.629305439856167,-0.30527573347708,
-0.873412008702649));
#19168=CARTESIAN_POINT('Ctrl Pts',(0.585840553788742,-0.29104845371857,
-0.903141581680914));
#19169=CARTESIAN_POINT('Ctrl Pts',(0.564362943424239,-0.28018331644634,
-0.916597376014514));
#19170=CARTESIAN_POINT('Ctrl Pts',(0.525933334162556,-0.254319232363049,
-0.939198248544427));
#19171=CARTESIAN_POINT('Ctrl Pts',(0.507057380724533,-0.237895043532788,
-0.949440676105255));
#19172=CARTESIAN_POINT('Ctrl Pts',(0.473077587363686,-0.199697230012983,
-0.966820759530997));
#19173=CARTESIAN_POINT('Ctrl Pts',(0.457978755888596,-0.177924977804098,
-0.973971221090534));
#19174=CARTESIAN_POINT('Ctrl Pts',(0.430199341854858,-0.124911173756694,
-0.986608710139579));
#19175=CARTESIAN_POINT('Ctrl Pts',(0.419070565453384,-0.0925528133349865,
-0.991263089003441));
#19176=CARTESIAN_POINT('Ctrl Pts',(0.413083465285518,-0.05953,-0.993751811093549));
#19177=CARTESIAN_POINT('Origin',(0.685838782044607,-0.05953,-0.860014630714833));
#19178=CARTESIAN_POINT('Origin',(0.,-0.208355,0.));
#19179=CARTESIAN_POINT('',(-1.076188,-0.35718,1.31795018948079E-16));
#19180=CARTESIAN_POINT('Origin',(0.,-0.35718,0.));
#19181=CARTESIAN_POINT('',(-1.076188,-0.208355,1.31795018948079E-16));
#19182=CARTESIAN_POINT('',(1.03449977959455,-0.05953,0.296632461748266));
#19183=CARTESIAN_POINT('Origin',(0.,-0.05953,0.));
#19184=CARTESIAN_POINT('',(1.03449977959455,-0.05953,-0.296632461748266));
#19185=CARTESIAN_POINT('Ctrl Pts',(1.03449977959455,-0.05953,0.296632461748267));
#19186=CARTESIAN_POINT('Ctrl Pts',(1.03628691421076,-0.0925528133349865,
0.290399865505497));
#19187=CARTESIAN_POINT('Ctrl Pts',(1.03958665287714,-0.124911173756694,
0.278797079997872));
#19188=CARTESIAN_POINT('Ctrl Pts',(1.0470264474309,-0.177924977804098,0.249198913998601));
#19189=CARTESIAN_POINT('Ctrl Pts',(1.05084995891418,-0.199697230012983,
0.232935932341942));
#19190=CARTESIAN_POINT('Ctrl Pts',(1.05844771715377,-0.237895043532788,
0.195533155353269));
#19191=CARTESIAN_POINT('Ctrl Pts',(1.06220882929878,-0.254319232363049,
0.17438929156337));
#19192=CARTESIAN_POINT('Ctrl Pts',(1.06849922508772,-0.28018331644634,0.130252399648131));
#19193=CARTESIAN_POINT('Ctrl Pts',(1.07137013248666,-0.29104845371857,0.105070977154072));
#19194=CARTESIAN_POINT('Ctrl Pts',(1.07522652957392,-0.30527573347708,0.0525526752791107));
#19195=CARTESIAN_POINT('Ctrl Pts',(1.076188,-0.308638795020976,0.025214283908933));
#19196=CARTESIAN_POINT('Ctrl Pts',(1.076188,-0.308638795020976,-0.025214283908933));
#19197=CARTESIAN_POINT('Ctrl Pts',(1.07522652957392,-0.30527573347708,-0.0525526752791107));
#19198=CARTESIAN_POINT('Ctrl Pts',(1.07137013248666,-0.29104845371857,-0.105070977154072));
#19199=CARTESIAN_POINT('Ctrl Pts',(1.06849922508772,-0.28018331644634,-0.130252399648131));
#19200=CARTESIAN_POINT('Ctrl Pts',(1.06220882929878,-0.254319232363049,
-0.17438929156337));
#19201=CARTESIAN_POINT('Ctrl Pts',(1.05844771715377,-0.237895043532788,
-0.195533155353269));
#19202=CARTESIAN_POINT('Ctrl Pts',(1.05084995891418,-0.199697230012983,
-0.232935932341942));
#19203=CARTESIAN_POINT('Ctrl Pts',(1.0470264474309,-0.177924977804098,-0.249198913998601));
#19204=CARTESIAN_POINT('Ctrl Pts',(1.03958665287714,-0.124911173756694,
-0.278797079997872));
#19205=CARTESIAN_POINT('Ctrl Pts',(1.03628691421076,-0.0925528133349865,
-0.290399865505497));
#19206=CARTESIAN_POINT('Ctrl Pts',(1.03449977959455,-0.05953,-0.296632461748267));
#19207=CARTESIAN_POINT('Origin',(0.,-0.05953,0.));
#19208=CARTESIAN_POINT('Origin',(0.,-0.05953,0.));
#19209=CARTESIAN_POINT('Origin',(1.1,-0.05953,0.));
#19210=CARTESIAN_POINT('Origin',(1.1,0.,0.));
#19211=CARTESIAN_POINT('Origin',(1.1,-0.05953,0.));
#19212=CARTESIAN_POINT('Origin',(0.,-0.35718,0.));
#19213=CARTESIAN_POINT('Origin',(0.,-0.05953,0.));
#19214=CARTESIAN_POINT('',(0.,0.,0.));
#19215=CARTESIAN_POINT('Origin',(1.119765,0.495,0.));
#19216=CARTESIAN_POINT('',(-1.119765,0.495,-1.37131662304724E-16));
#19217=CARTESIAN_POINT('Origin',(0.,0.495,0.));
#19218=CARTESIAN_POINT('',(-1.085235,0.495,-1.32902956907268E-16));
#19219=CARTESIAN_POINT('Origin',(0.,0.495,0.));
#19220=CARTESIAN_POINT('Origin',(0.,0.4575,0.));
#19221=CARTESIAN_POINT('',(-1.119765,0.42,-1.37131662304724E-16));
#19222=CARTESIAN_POINT('Origin',(0.,0.42,0.));
#19223=CARTESIAN_POINT('',(-1.119765,0.4575,-1.37131662304724E-16));
#19224=CARTESIAN_POINT('Origin',(1.085235,0.42,0.));
#19225=CARTESIAN_POINT('',(-1.085235,0.42,-1.32902956907268E-16));
#19226=CARTESIAN_POINT('Origin',(0.,0.42,0.));
#19227=CARTESIAN_POINT('Origin',(0.,0.4575,0.));
#19228=CARTESIAN_POINT('',(-1.085235,0.4575,-1.32902956907268E-16));
#19229=CARTESIAN_POINT('Origin',(1.119765,-0.42,0.));
#19230=CARTESIAN_POINT('',(-1.119765,-0.42,-1.37131662304724E-16));
#19231=CARTESIAN_POINT('Origin',(0.,-0.42,0.));
#19232=CARTESIAN_POINT('',(-1.085235,-0.42,-1.32902956907268E-16));
#19233=CARTESIAN_POINT('Origin',(0.,-0.42,0.));
#19234=CARTESIAN_POINT('Origin',(0.,-0.4575,0.));
#19235=CARTESIAN_POINT('',(-1.119765,-0.495,-1.37131662304724E-16));
#19236=CARTESIAN_POINT('Origin',(0.,-0.495,0.));
#19237=CARTESIAN_POINT('',(-1.119765,-0.4575,-1.37131662304724E-16));
#19238=CARTESIAN_POINT('Origin',(1.085235,-0.495,0.));
#19239=CARTESIAN_POINT('',(-1.085235,-0.495,-1.32902956907268E-16));
#19240=CARTESIAN_POINT('Origin',(0.,-0.495,0.));
#19241=CARTESIAN_POINT('Origin',(0.,-0.4575,0.));
#19242=CARTESIAN_POINT('',(-1.085235,-0.4575,-1.32902956907268E-16));
#19243=CARTESIAN_POINT('',(0.,0.,0.));
#19244=CARTESIAN_POINT('',(0.,0.,0.));
#19245=CARTESIAN_POINT('',(0.,0.,0.));
#19246=CARTESIAN_POINT('',(0.,0.,0.));
#19247=CARTESIAN_POINT('',(0.,0.,0.));
#19248=CARTESIAN_POINT('',(0.,0.,0.));
#19249=CARTESIAN_POINT('Origin',(0.0866025403784439,-0.4,-0.15));
#19250=CARTESIAN_POINT('',(0.173205080756888,-0.4,0.));
#19251=CARTESIAN_POINT('',(0.0866025403784439,-0.4,-0.15));
#19252=CARTESIAN_POINT('',(0.173205080756888,-0.4,0.));
#19253=CARTESIAN_POINT('',(0.0866025403784439,-0.64,-0.15));
#19254=CARTESIAN_POINT('',(0.0866025403784439,-0.4,-0.15));
#19255=CARTESIAN_POINT('',(0.173205080756888,-0.64,0.));
#19256=CARTESIAN_POINT('',(0.173205080756888,-0.64,0.));
#19257=CARTESIAN_POINT('',(0.173205080756888,-0.4,0.));
#19258=CARTESIAN_POINT('Origin',(-0.0866025403784438,-0.4,-0.15));
#19259=CARTESIAN_POINT('',(-0.0866025403784438,-0.4,-0.15));
#19260=CARTESIAN_POINT('',(0.0866025403784439,-0.4,-0.15));
#19261=CARTESIAN_POINT('',(-0.0866025403784438,-0.64,-0.15));
#19262=CARTESIAN_POINT('',(-0.0866025403784438,-0.4,-0.15));
#19263=CARTESIAN_POINT('',(0.0866025403784439,-0.64,-0.15));
#19264=CARTESIAN_POINT('Origin',(-0.173205080756888,-0.4,-2.77555756156289E-17));
#19265=CARTESIAN_POINT('',(-0.173205080756888,-0.4,-2.12115047744981E-17));
#19266=CARTESIAN_POINT('',(-0.0866025403784438,-0.4,-0.15));
#19267=CARTESIAN_POINT('',(-0.173205080756888,-0.64,-2.77555756156289E-17));
#19268=CARTESIAN_POINT('',(-0.173205080756888,-0.4,-2.12115047744981E-17));
#19269=CARTESIAN_POINT('',(-0.0866025403784438,-0.64,-0.15));
#19270=CARTESIAN_POINT('Origin',(-0.0866025403784439,-0.4,0.15));
#19271=CARTESIAN_POINT('',(-0.0866025403784439,-0.4,0.15));
#19272=CARTESIAN_POINT('',(-0.173205080756888,-0.4,-2.12115047744981E-17));
#19273=CARTESIAN_POINT('',(-0.0866025403784439,-0.64,0.15));
#19274=CARTESIAN_POINT('',(-0.0866025403784439,-0.4,0.15));
#19275=CARTESIAN_POINT('',(-0.173205080756888,-0.64,-2.12115047744981E-17));
#19276=CARTESIAN_POINT('Origin',(0.0866025403784439,-0.4,0.15));
#19277=CARTESIAN_POINT('',(0.0866025403784439,-0.4,0.15));
#19278=CARTESIAN_POINT('',(-0.0866025403784439,-0.4,0.15));
#19279=CARTESIAN_POINT('',(0.0866025403784439,-0.64,0.15));
#19280=CARTESIAN_POINT('',(0.0866025403784439,-0.4,0.15));
#19281=CARTESIAN_POINT('',(-0.0866025403784439,-0.64,0.15));
#19282=CARTESIAN_POINT('Origin',(0.173205080756888,-0.4,0.));
#19283=CARTESIAN_POINT('',(0.0866025403784439,-0.4,0.15));
#19284=CARTESIAN_POINT('',(0.0866025403784439,-0.64,0.15));
#19285=CARTESIAN_POINT('Origin',(0.,-0.4,-2.77555756156289E-17));
#19286=CARTESIAN_POINT('Origin',(0.,-0.64,-2.77555756156289E-17));
#19287=CARTESIAN_POINT('Origin',(0.,-1.,0.));
#19288=CARTESIAN_POINT('',(-0.1954,-1.,2.39295984553393E-17));
#19289=CARTESIAN_POINT('Origin',(0.,-1.,0.));
#19290=CARTESIAN_POINT('Origin',(0.3,0.4,0.));
#19291=CARTESIAN_POINT('',(-0.3,0.4,-3.67394039744206E-17));
#19292=CARTESIAN_POINT('Origin',(0.,0.4,0.));
#19293=CARTESIAN_POINT('Origin',(0.,0.375,0.));
#19294=CARTESIAN_POINT('',(-0.35,0.35,-4.28626379701573E-17));
#19295=CARTESIAN_POINT('Origin',(0.,0.35,0.));
#19296=CARTESIAN_POINT('',(-0.325,0.375,-3.9801020972289E-17));
#19297=CARTESIAN_POINT('Origin',(0.,0.19,0.));
#19298=CARTESIAN_POINT('',(-0.35,0.03,-4.28626379701574E-17));
#19299=CARTESIAN_POINT('Origin',(0.,0.03,0.));
#19300=CARTESIAN_POINT('',(-0.35,0.19,-4.28626379701574E-17));
#19301=CARTESIAN_POINT('Origin',(0.,0.0149999999999999,0.));
#19302=CARTESIAN_POINT('',(-0.32,-3.29597460435593E-17,-3.91886975727153E-17));
#19303=CARTESIAN_POINT('Origin',(0.,0.,0.));
#19304=CARTESIAN_POINT('',(-0.335,0.0149999999999999,-4.10256677714363E-17));
#19305=CARTESIAN_POINT('Origin',(0.22,0.,0.));
#19306=CARTESIAN_POINT('',(-0.22,-6.93889390390723E-18,-2.69422295812418E-17));
#19307=CARTESIAN_POINT('Origin',(0.,0.,0.));
#19308=CARTESIAN_POINT('Origin',(0.,-0.02,0.));
#19309=CARTESIAN_POINT('',(-0.1954,-0.0492,2.39295984553393E-17));
#19310=CARTESIAN_POINT('Origin',(0.,-0.0492,0.));
#19311=CARTESIAN_POINT('',(-0.21,-0.02,-2.57175827820944E-17));
#19312=CARTESIAN_POINT('Origin',(0.,-0.8,0.));
#19313=CARTESIAN_POINT('',(-0.1954,-0.8,-2.39295984553393E-17));
#19314=CARTESIAN_POINT('',(0.,0.,0.));
#19315=CARTESIAN_POINT('',(0.,0.,0.));
#19316=CARTESIAN_POINT('Origin',(1.,0.,10.7));
#19317=CARTESIAN_POINT('',(0.575,-5.20474889637625E-17,10.8));
#19318=CARTESIAN_POINT('Origin',(1.,0.,10.8));
#19319=CARTESIAN_POINT('',(0.575,-5.20474889637625E-17,12.));
#19320=CARTESIAN_POINT('',(0.575,-5.20474889637625E-17,10.7));
#19321=CARTESIAN_POINT('Origin',(1.,0.,12.));
#19322=CARTESIAN_POINT('Origin',(1.,0.,12.));
#19323=CARTESIAN_POINT('Origin',(0.2,-1.,37.));
#19324=CARTESIAN_POINT('',(0.2,-0.6,37.));
#19325=CARTESIAN_POINT('',(0.2,-0.6,11.));
#19326=CARTESIAN_POINT('',(0.2,-0.6,10.8));
#19327=CARTESIAN_POINT('',(0.2,-1.,37.));
#19328=CARTESIAN_POINT('',(0.2,-1.,37.));
#19329=CARTESIAN_POINT('',(0.2,-1.,11.));
#19330=CARTESIAN_POINT('',(0.2,-1.,11.));
#19331=CARTESIAN_POINT('',(0.2,-1.,11.));
#19332=CARTESIAN_POINT('Origin',(0.2,-1.,37.));
#19333=CARTESIAN_POINT('',(0.2,0.6,11.));
#19334=CARTESIAN_POINT('',(0.2,0.6,37.));
#19335=CARTESIAN_POINT('',(0.2,0.6,10.8));
#19336=CARTESIAN_POINT('',(0.2,1.,11.));
#19337=CARTESIAN_POINT('',(0.2,-1.,11.));
#19338=CARTESIAN_POINT('',(0.2,1.,37.));
#19339=CARTESIAN_POINT('',(0.2,1.,11.));
#19340=CARTESIAN_POINT('',(0.2,-1.,37.));
#19341=CARTESIAN_POINT('Origin',(0.2,-1.,11.));
#19342=CARTESIAN_POINT('',(0.,-1.22464679914735E-16,11.));
#19343=CARTESIAN_POINT('Origin',(1.,0.,11.));
#19344=CARTESIAN_POINT('',(-1.,-1.,11.));
#19345=CARTESIAN_POINT('',(-1.,-1.,11.));
#19346=CARTESIAN_POINT('',(-1.,1.,11.));
#19347=CARTESIAN_POINT('',(-1.,-1.,11.));
#19348=CARTESIAN_POINT('',(-1.,1.,11.));
#19349=CARTESIAN_POINT('Origin',(1.,0.,11.));
#19350=CARTESIAN_POINT('Origin',(-1.,-1.,37.));
#19351=CARTESIAN_POINT('',(0.,-1.22464679914735E-16,37.));
#19352=CARTESIAN_POINT('Origin',(1.,0.,37.));
#19353=CARTESIAN_POINT('',(-1.,1.,37.));
#19354=CARTESIAN_POINT('',(0.2,1.,37.));
#19355=CARTESIAN_POINT('',(-1.,-1.,37.));
#19356=CARTESIAN_POINT('',(-1.,-1.,37.));
#19357=CARTESIAN_POINT('',(0.2,-1.,37.));
#19358=CARTESIAN_POINT('Origin',(1.,0.,37.));
#19359=CARTESIAN_POINT('Origin',(-1.,-1.,36.269194724554));
#19360=CARTESIAN_POINT('',(-1.,-1.,36.269194724554));
#19361=CARTESIAN_POINT('',(-1.,-1.,37.));
#19362=CARTESIAN_POINT('',(-1.,1.,36.269194724554));
#19363=CARTESIAN_POINT('',(-1.,1.,37.));
#19364=CARTESIAN_POINT('',(-1.,-1.,36.269194724554));
#19365=CARTESIAN_POINT('Origin',(-1.45,-1.,36.1054081191342));
#19366=CARTESIAN_POINT('',(-1.45,-1.,36.1054081191342));
#19367=CARTESIAN_POINT('',(-1.,-1.,36.269194724554));
#19368=CARTESIAN_POINT('',(-1.45,1.,36.1054081191342));
#19369=CARTESIAN_POINT('',(-1.,1.,36.269194724554));
#19370=CARTESIAN_POINT('',(-1.45,-1.,36.1054081191342));
#19371=CARTESIAN_POINT('Origin',(-1.45,-1.,35.9388369474817));
#19372=CARTESIAN_POINT('',(-1.45,-1.,35.9388369474817));
#19373=CARTESIAN_POINT('',(-1.45,-1.,36.1054081191342));
#19374=CARTESIAN_POINT('',(-1.45,1.,35.9388369474817));
#19375=CARTESIAN_POINT('',(-1.45,1.,36.1054081191342));
#19376=CARTESIAN_POINT('',(-1.45,-1.,35.9388369474817));
#19377=CARTESIAN_POINT('Origin',(-1.,-1.,35.7750503420619));
#19378=CARTESIAN_POINT('',(-1.,-1.,35.7750503420619));
#19379=CARTESIAN_POINT('',(-1.45,-1.,35.9388369474817));
#19380=CARTESIAN_POINT('',(-1.,1.,35.7750503420619));
#19381=CARTESIAN_POINT('',(-1.45,1.,35.9388369474817));
#19382=CARTESIAN_POINT('',(-1.,-1.,35.7750503420619));
#19383=CARTESIAN_POINT('Origin',(-1.,-1.,35.640876193836));
#19384=CARTESIAN_POINT('',(-1.,-1.,35.640876193836));
#19385=CARTESIAN_POINT('',(-1.,-1.,35.7750503420619));
#19386=CARTESIAN_POINT('',(-1.,1.,35.640876193836));
#19387=CARTESIAN_POINT('',(-1.,1.,35.7750503420619));
#19388=CARTESIAN_POINT('',(-1.,-1.,35.640876193836));
#19389=CARTESIAN_POINT('Origin',(-1.45,-1.,35.4770895884162));
#19390=CARTESIAN_POINT('',(-1.45,-1.,35.4770895884162));
#19391=CARTESIAN_POINT('',(-1.,-1.,35.640876193836));
#19392=CARTESIAN_POINT('',(-1.45,1.,35.4770895884162));
#19393=CARTESIAN_POINT('',(-1.,1.,35.640876193836));
#19394=CARTESIAN_POINT('',(-1.45,-1.,35.4770895884162));
#19395=CARTESIAN_POINT('Origin',(-1.45,-1.,35.3105184167637));
#19396=CARTESIAN_POINT('',(-1.45,-1.,35.3105184167637));
#19397=CARTESIAN_POINT('',(-1.45,-1.,35.4770895884162));
#19398=CARTESIAN_POINT('',(-1.45,1.,35.3105184167637));
#19399=CARTESIAN_POINT('',(-1.45,1.,35.4770895884162));
#19400=CARTESIAN_POINT('',(-1.45,-1.,35.3105184167637));
#19401=CARTESIAN_POINT('Origin',(-1.,-1.,35.1467318113439));
#19402=CARTESIAN_POINT('',(-1.,-1.,35.1467318113439));
#19403=CARTESIAN_POINT('',(-1.45,-1.,35.3105184167637));
#19404=CARTESIAN_POINT('',(-1.,1.,35.1467318113439));
#19405=CARTESIAN_POINT('',(-1.45,1.,35.3105184167637));
#19406=CARTESIAN_POINT('',(-1.,-1.,35.1467318113439));
#19407=CARTESIAN_POINT('Origin',(-1.,-1.,35.0125576631181));
#19408=CARTESIAN_POINT('',(-1.,-1.,35.0125576631181));
#19409=CARTESIAN_POINT('',(-1.,-1.,35.1467318113439));
#19410=CARTESIAN_POINT('',(-1.,1.,35.0125576631181));
#19411=CARTESIAN_POINT('',(-1.,1.,35.1467318113439));
#19412=CARTESIAN_POINT('',(-1.,-1.,35.0125576631181));
#19413=CARTESIAN_POINT('Origin',(-1.45,-1.,34.8487710576983));
#19414=CARTESIAN_POINT('',(-1.45,-1.,34.8487710576983));
#19415=CARTESIAN_POINT('',(-1.,-1.,35.0125576631181));
#19416=CARTESIAN_POINT('',(-1.45,1.,34.8487710576983));
#19417=CARTESIAN_POINT('',(-1.,1.,35.0125576631181));
#19418=CARTESIAN_POINT('',(-1.45,-1.,34.8487710576983));
#19419=CARTESIAN_POINT('Origin',(-1.45,-1.,34.6821998860458));
#19420=CARTESIAN_POINT('',(-1.45,-1.,34.6821998860458));
#19421=CARTESIAN_POINT('',(-1.45,-1.,34.8487710576983));
#19422=CARTESIAN_POINT('',(-1.45,1.,34.6821998860458));
#19423=CARTESIAN_POINT('',(-1.45,1.,34.8487710576983));
#19424=CARTESIAN_POINT('',(-1.45,-1.,34.6821998860458));
#19425=CARTESIAN_POINT('Origin',(-1.,-1.,34.518413280626));
#19426=CARTESIAN_POINT('',(-1.,-1.,34.518413280626));
#19427=CARTESIAN_POINT('',(-1.45,-1.,34.6821998860458));
#19428=CARTESIAN_POINT('',(-1.,1.,34.518413280626));
#19429=CARTESIAN_POINT('',(-1.45,1.,34.6821998860458));
#19430=CARTESIAN_POINT('',(-1.,-1.,34.518413280626));
#19431=CARTESIAN_POINT('Origin',(-1.,-1.,34.3842391324001));
#19432=CARTESIAN_POINT('',(-1.,-1.,34.3842391324001));
#19433=CARTESIAN_POINT('',(-1.,-1.,34.518413280626));
#19434=CARTESIAN_POINT('',(-1.,1.,34.3842391324001));
#19435=CARTESIAN_POINT('',(-1.,1.,34.518413280626));
#19436=CARTESIAN_POINT('',(-1.,-1.,34.3842391324001));
#19437=CARTESIAN_POINT('Origin',(-1.45,-1.,34.2204525269803));
#19438=CARTESIAN_POINT('',(-1.45,-1.,34.2204525269803));
#19439=CARTESIAN_POINT('',(-1.,-1.,34.3842391324001));
#19440=CARTESIAN_POINT('',(-1.45,1.,34.2204525269803));
#19441=CARTESIAN_POINT('',(-1.,1.,34.3842391324001));
#19442=CARTESIAN_POINT('',(-1.45,-1.,34.2204525269803));
#19443=CARTESIAN_POINT('Origin',(-1.45,-1.,34.0538813553278));
#19444=CARTESIAN_POINT('',(-1.45,-1.,34.0538813553278));
#19445=CARTESIAN_POINT('',(-1.45,-1.,34.2204525269803));
#19446=CARTESIAN_POINT('',(-1.45,1.,34.0538813553278));
#19447=CARTESIAN_POINT('',(-1.45,1.,34.2204525269803));
#19448=CARTESIAN_POINT('',(-1.45,-1.,34.0538813553278));
#19449=CARTESIAN_POINT('Origin',(-1.,-1.,33.890094749908));
#19450=CARTESIAN_POINT('',(-1.,-1.,33.890094749908));
#19451=CARTESIAN_POINT('',(-1.45,-1.,34.0538813553278));
#19452=CARTESIAN_POINT('',(-1.,1.,33.890094749908));
#19453=CARTESIAN_POINT('',(-1.45,1.,34.0538813553278));
#19454=CARTESIAN_POINT('',(-1.,-1.,33.890094749908));
#19455=CARTESIAN_POINT('Origin',(-1.,-1.,33.7559206016821));
#19456=CARTESIAN_POINT('',(-1.,-1.,33.7559206016821));
#19457=CARTESIAN_POINT('',(-1.,-1.,33.890094749908));
#19458=CARTESIAN_POINT('',(-1.,1.,33.7559206016821));
#19459=CARTESIAN_POINT('',(-1.,1.,33.890094749908));
#19460=CARTESIAN_POINT('',(-1.,-1.,33.7559206016821));
#19461=CARTESIAN_POINT('Origin',(-1.45,-1.,33.5921339962624));
#19462=CARTESIAN_POINT('',(-1.45,-1.,33.5921339962624));
#19463=CARTESIAN_POINT('',(-1.,-1.,33.7559206016821));
#19464=CARTESIAN_POINT('',(-1.45,1.,33.5921339962624));
#19465=CARTESIAN_POINT('',(-1.,1.,33.7559206016821));
#19466=CARTESIAN_POINT('',(-1.45,-1.,33.5921339962624));
#19467=CARTESIAN_POINT('Origin',(-1.45,-1.,33.4255628246099));
#19468=CARTESIAN_POINT('',(-1.45,-1.,33.4255628246099));
#19469=CARTESIAN_POINT('',(-1.45,-1.,33.5921339962624));
#19470=CARTESIAN_POINT('',(-1.45,1.,33.4255628246099));
#19471=CARTESIAN_POINT('',(-1.45,1.,33.5921339962624));
#19472=CARTESIAN_POINT('',(-1.45,-1.,33.4255628246099));
#19473=CARTESIAN_POINT('Origin',(-1.,-1.,33.2617762191901));
#19474=CARTESIAN_POINT('',(-1.,-1.,33.2617762191901));
#19475=CARTESIAN_POINT('',(-1.45,-1.,33.4255628246099));
#19476=CARTESIAN_POINT('',(-1.,1.,33.2617762191901));
#19477=CARTESIAN_POINT('',(-1.45,1.,33.4255628246099));
#19478=CARTESIAN_POINT('',(-1.,-1.,33.2617762191901));
#19479=CARTESIAN_POINT('Origin',(-1.,-1.,33.1276020709642));
#19480=CARTESIAN_POINT('',(-1.,-1.,33.1276020709642));
#19481=CARTESIAN_POINT('',(-1.,-1.,33.2617762191901));
#19482=CARTESIAN_POINT('',(-1.,1.,33.1276020709642));
#19483=CARTESIAN_POINT('',(-1.,1.,33.2617762191901));
#19484=CARTESIAN_POINT('',(-1.,-1.,33.1276020709642));
#19485=CARTESIAN_POINT('Origin',(-1.45,-1.,32.9638154655444));
#19486=CARTESIAN_POINT('',(-1.45,-1.,32.9638154655444));
#19487=CARTESIAN_POINT('',(-1.,-1.,33.1276020709642));
#19488=CARTESIAN_POINT('',(-1.45,1.,32.9638154655444));
#19489=CARTESIAN_POINT('',(-1.,1.,33.1276020709642));
#19490=CARTESIAN_POINT('',(-1.45,-1.,32.9638154655444));
#19491=CARTESIAN_POINT('Origin',(-1.45,-1.,32.7972442938919));
#19492=CARTESIAN_POINT('',(-1.45,-1.,32.7972442938919));
#19493=CARTESIAN_POINT('',(-1.45,-1.,32.9638154655444));
#19494=CARTESIAN_POINT('',(-1.45,1.,32.7972442938919));
#19495=CARTESIAN_POINT('',(-1.45,1.,32.9638154655444));
#19496=CARTESIAN_POINT('',(-1.45,-1.,32.7972442938919));
#19497=CARTESIAN_POINT('Origin',(-1.,-1.,32.6334576884721));
#19498=CARTESIAN_POINT('',(-1.,-1.,32.6334576884721));
#19499=CARTESIAN_POINT('',(-1.45,-1.,32.7972442938919));
#19500=CARTESIAN_POINT('',(-1.,1.,32.6334576884721));
#19501=CARTESIAN_POINT('',(-1.45,1.,32.7972442938919));
#19502=CARTESIAN_POINT('',(-1.,-1.,32.6334576884721));
#19503=CARTESIAN_POINT('Origin',(-1.,-1.,32.4992835402462));
#19504=CARTESIAN_POINT('',(-1.,-1.,32.4992835402462));
#19505=CARTESIAN_POINT('',(-1.,-1.,32.6334576884721));
#19506=CARTESIAN_POINT('',(-1.,1.,32.4992835402462));
#19507=CARTESIAN_POINT('',(-1.,1.,32.6334576884721));
#19508=CARTESIAN_POINT('',(-1.,-1.,32.4992835402462));
#19509=CARTESIAN_POINT('Origin',(-1.45,-1.,32.3354969348264));
#19510=CARTESIAN_POINT('',(-1.45,-1.,32.3354969348264));
#19511=CARTESIAN_POINT('',(-1.,-1.,32.4992835402462));
#19512=CARTESIAN_POINT('',(-1.45,1.,32.3354969348264));
#19513=CARTESIAN_POINT('',(-1.,1.,32.4992835402462));
#19514=CARTESIAN_POINT('',(-1.45,-1.,32.3354969348264));
#19515=CARTESIAN_POINT('Origin',(-1.45,-1.,32.1689257631739));
#19516=CARTESIAN_POINT('',(-1.45,-1.,32.1689257631739));
#19517=CARTESIAN_POINT('',(-1.45,-1.,32.3354969348264));
#19518=CARTESIAN_POINT('',(-1.45,1.,32.1689257631739));
#19519=CARTESIAN_POINT('',(-1.45,1.,32.3354969348264));
#19520=CARTESIAN_POINT('',(-1.45,-1.,32.1689257631739));
#19521=CARTESIAN_POINT('Origin',(-1.,-1.,32.0051391577542));
#19522=CARTESIAN_POINT('',(-1.,-1.,32.0051391577542));
#19523=CARTESIAN_POINT('',(-1.45,-1.,32.1689257631739));
#19524=CARTESIAN_POINT('',(-1.,1.,32.0051391577542));
#19525=CARTESIAN_POINT('',(-1.45,1.,32.1689257631739));
#19526=CARTESIAN_POINT('',(-1.,-1.,32.0051391577542));
#19527=CARTESIAN_POINT('Origin',(-1.,-1.,31.8709650095283));
#19528=CARTESIAN_POINT('',(-1.,-1.,31.8709650095283));
#19529=CARTESIAN_POINT('',(-1.,-1.,32.0051391577542));
#19530=CARTESIAN_POINT('',(-1.,1.,31.8709650095283));
#19531=CARTESIAN_POINT('',(-1.,1.,32.0051391577542));
#19532=CARTESIAN_POINT('',(-1.,-1.,31.8709650095283));
#19533=CARTESIAN_POINT('Origin',(-1.45,-1.,31.7071784041085));
#19534=CARTESIAN_POINT('',(-1.45,-1.,31.7071784041085));
#19535=CARTESIAN_POINT('',(-1.,-1.,31.8709650095283));
#19536=CARTESIAN_POINT('',(-1.45,1.,31.7071784041085));
#19537=CARTESIAN_POINT('',(-1.,1.,31.8709650095283));
#19538=CARTESIAN_POINT('',(-1.45,-1.,31.7071784041085));
#19539=CARTESIAN_POINT('Origin',(-1.45,-1.,31.540607232456));
#19540=CARTESIAN_POINT('',(-1.45,-1.,31.540607232456));
#19541=CARTESIAN_POINT('',(-1.45,-1.,31.7071784041085));
#19542=CARTESIAN_POINT('',(-1.45,1.,31.540607232456));
#19543=CARTESIAN_POINT('',(-1.45,1.,31.7071784041085));
#19544=CARTESIAN_POINT('',(-1.45,-1.,31.540607232456));
#19545=CARTESIAN_POINT('Origin',(-1.,-1.,31.3768206270362));
#19546=CARTESIAN_POINT('',(-1.,-1.,31.3768206270362));
#19547=CARTESIAN_POINT('',(-1.45,-1.,31.540607232456));
#19548=CARTESIAN_POINT('',(-1.,1.,31.3768206270362));
#19549=CARTESIAN_POINT('',(-1.45,1.,31.540607232456));
#19550=CARTESIAN_POINT('',(-1.,-1.,31.3768206270362));
#19551=CARTESIAN_POINT('Origin',(-1.,-1.,31.2426464788103));
#19552=CARTESIAN_POINT('',(-1.,-1.,31.2426464788103));
#19553=CARTESIAN_POINT('',(-1.,-1.,31.3768206270362));
#19554=CARTESIAN_POINT('',(-1.,1.,31.2426464788103));
#19555=CARTESIAN_POINT('',(-1.,1.,31.3768206270362));
#19556=CARTESIAN_POINT('',(-1.,-1.,31.2426464788103));
#19557=CARTESIAN_POINT('Origin',(-1.45,-1.,31.0788598733905));
#19558=CARTESIAN_POINT('',(-1.45,-1.,31.0788598733905));
#19559=CARTESIAN_POINT('',(-1.,-1.,31.2426464788103));
#19560=CARTESIAN_POINT('',(-1.45,1.,31.0788598733905));
#19561=CARTESIAN_POINT('',(-1.,1.,31.2426464788103));
#19562=CARTESIAN_POINT('',(-1.45,-1.,31.0788598733905));
#19563=CARTESIAN_POINT('Origin',(-1.45,-1.,30.912288701738));
#19564=CARTESIAN_POINT('',(-1.45,-1.,30.912288701738));
#19565=CARTESIAN_POINT('',(-1.45,-1.,31.0788598733905));
#19566=CARTESIAN_POINT('',(-1.45,1.,30.912288701738));
#19567=CARTESIAN_POINT('',(-1.45,1.,31.0788598733905));
#19568=CARTESIAN_POINT('',(-1.45,-1.,30.912288701738));
#19569=CARTESIAN_POINT('Origin',(-1.,-1.,30.7485020963182));
#19570=CARTESIAN_POINT('',(-1.,-1.,30.7485020963182));
#19571=CARTESIAN_POINT('',(-1.45,-1.,30.912288701738));
#19572=CARTESIAN_POINT('',(-1.,1.,30.7485020963182));
#19573=CARTESIAN_POINT('',(-1.45,1.,30.912288701738));
#19574=CARTESIAN_POINT('',(-1.,-1.,30.7485020963182));
#19575=CARTESIAN_POINT('Origin',(-1.,-1.,30.6143279480924));
#19576=CARTESIAN_POINT('',(-1.,-1.,30.6143279480924));
#19577=CARTESIAN_POINT('',(-1.,-1.,30.7485020963182));
#19578=CARTESIAN_POINT('',(-1.,1.,30.6143279480924));
#19579=CARTESIAN_POINT('',(-1.,1.,30.7485020963182));
#19580=CARTESIAN_POINT('',(-1.,-1.,30.6143279480924));
#19581=CARTESIAN_POINT('Origin',(-1.45,-1.,30.4505413426726));
#19582=CARTESIAN_POINT('',(-1.45,-1.,30.4505413426726));
#19583=CARTESIAN_POINT('',(-1.,-1.,30.6143279480924));
#19584=CARTESIAN_POINT('',(-1.45,1.,30.4505413426726));
#19585=CARTESIAN_POINT('',(-1.,1.,30.6143279480924));
#19586=CARTESIAN_POINT('',(-1.45,-1.,30.4505413426726));
#19587=CARTESIAN_POINT('Origin',(-1.45,-1.,30.2839701710201));
#19588=CARTESIAN_POINT('',(-1.45,-1.,30.2839701710201));
#19589=CARTESIAN_POINT('',(-1.45,-1.,30.4505413426726));
#19590=CARTESIAN_POINT('',(-1.45,1.,30.2839701710201));
#19591=CARTESIAN_POINT('',(-1.45,1.,30.4505413426726));
#19592=CARTESIAN_POINT('',(-1.45,-1.,30.2839701710201));
#19593=CARTESIAN_POINT('Origin',(-1.,-1.,30.1201835656003));
#19594=CARTESIAN_POINT('',(-1.,-1.,30.1201835656003));
#19595=CARTESIAN_POINT('',(-1.45,-1.,30.2839701710201));
#19596=CARTESIAN_POINT('',(-1.,1.,30.1201835656003));
#19597=CARTESIAN_POINT('',(-1.45,1.,30.2839701710201));
#19598=CARTESIAN_POINT('',(-1.,-1.,30.1201835656003));
#19599=CARTESIAN_POINT('Origin',(-1.,-1.,29.9860094173744));
#19600=CARTESIAN_POINT('',(-1.,-1.,29.9860094173744));
#19601=CARTESIAN_POINT('',(-1.,-1.,30.1201835656003));
#19602=CARTESIAN_POINT('',(-1.,1.,29.9860094173744));
#19603=CARTESIAN_POINT('',(-1.,1.,30.1201835656003));
#19604=CARTESIAN_POINT('',(-1.,-1.,29.9860094173744));
#19605=CARTESIAN_POINT('Origin',(-1.45,-1.,29.8222228119546));
#19606=CARTESIAN_POINT('',(-1.45,-1.,29.8222228119546));
#19607=CARTESIAN_POINT('',(-1.,-1.,29.9860094173744));
#19608=CARTESIAN_POINT('',(-1.45,1.,29.8222228119546));
#19609=CARTESIAN_POINT('',(-1.,1.,29.9860094173744));
#19610=CARTESIAN_POINT('',(-1.45,-1.,29.8222228119546));
#19611=CARTESIAN_POINT('Origin',(-1.45,-1.,29.6556516403021));
#19612=CARTESIAN_POINT('',(-1.45,-1.,29.6556516403021));
#19613=CARTESIAN_POINT('',(-1.45,-1.,29.8222228119546));
#19614=CARTESIAN_POINT('',(-1.45,1.,29.6556516403021));
#19615=CARTESIAN_POINT('',(-1.45,1.,29.8222228119546));
#19616=CARTESIAN_POINT('',(-1.45,-1.,29.6556516403021));
#19617=CARTESIAN_POINT('Origin',(-1.,-1.,29.4918650348823));
#19618=CARTESIAN_POINT('',(-1.,-1.,29.4918650348823));
#19619=CARTESIAN_POINT('',(-1.45,-1.,29.6556516403021));
#19620=CARTESIAN_POINT('',(-1.,1.,29.4918650348823));
#19621=CARTESIAN_POINT('',(-1.45,1.,29.6556516403021));
#19622=CARTESIAN_POINT('',(-1.,-1.,29.4918650348823));
#19623=CARTESIAN_POINT('Origin',(-1.,-1.,29.3576908866564));
#19624=CARTESIAN_POINT('',(-1.,-1.,29.3576908866564));
#19625=CARTESIAN_POINT('',(-1.,-1.,29.4918650348823));
#19626=CARTESIAN_POINT('',(-1.,1.,29.3576908866564));
#19627=CARTESIAN_POINT('',(-1.,1.,29.4918650348823));
#19628=CARTESIAN_POINT('',(-1.,-1.,29.3576908866564));
#19629=CARTESIAN_POINT('Origin',(-1.45,-1.,29.1939042812366));
#19630=CARTESIAN_POINT('',(-1.45,-1.,29.1939042812366));
#19631=CARTESIAN_POINT('',(-1.,-1.,29.3576908866564));
#19632=CARTESIAN_POINT('',(-1.45,1.,29.1939042812366));
#19633=CARTESIAN_POINT('',(-1.,1.,29.3576908866564));
#19634=CARTESIAN_POINT('',(-1.45,-1.,29.1939042812366));
#19635=CARTESIAN_POINT('Origin',(-1.45,-1.,29.0273331095841));
#19636=CARTESIAN_POINT('',(-1.45,-1.,29.0273331095841));
#19637=CARTESIAN_POINT('',(-1.45,-1.,29.1939042812366));
#19638=CARTESIAN_POINT('',(-1.45,1.,29.0273331095841));
#19639=CARTESIAN_POINT('',(-1.45,1.,29.1939042812366));
#19640=CARTESIAN_POINT('',(-1.45,-1.,29.0273331095841));
#19641=CARTESIAN_POINT('Origin',(-1.,-1.,28.8635465041644));
#19642=CARTESIAN_POINT('',(-1.,-1.,28.8635465041644));
#19643=CARTESIAN_POINT('',(-1.45,-1.,29.0273331095841));
#19644=CARTESIAN_POINT('',(-1.,1.,28.8635465041644));
#19645=CARTESIAN_POINT('',(-1.45,1.,29.0273331095841));
#19646=CARTESIAN_POINT('',(-1.,-1.,28.8635465041644));
#19647=CARTESIAN_POINT('Origin',(-1.,-1.,28.7293723559385));
#19648=CARTESIAN_POINT('',(-1.,-1.,28.7293723559385));
#19649=CARTESIAN_POINT('',(-1.,-1.,28.8635465041644));
#19650=CARTESIAN_POINT('',(-1.,1.,28.7293723559385));
#19651=CARTESIAN_POINT('',(-1.,1.,28.8635465041644));
#19652=CARTESIAN_POINT('',(-1.,-1.,28.7293723559385));
#19653=CARTESIAN_POINT('Origin',(-1.45,-1.,28.5655857505187));
#19654=CARTESIAN_POINT('',(-1.45,-1.,28.5655857505187));
#19655=CARTESIAN_POINT('',(-1.,-1.,28.7293723559385));
#19656=CARTESIAN_POINT('',(-1.45,1.,28.5655857505187));
#19657=CARTESIAN_POINT('',(-1.,1.,28.7293723559385));
#19658=CARTESIAN_POINT('',(-1.45,-1.,28.5655857505187));
#19659=CARTESIAN_POINT('Origin',(-1.45,-1.,28.3990145788662));
#19660=CARTESIAN_POINT('',(-1.45,-1.,28.3990145788662));
#19661=CARTESIAN_POINT('',(-1.45,-1.,28.5655857505187));
#19662=CARTESIAN_POINT('',(-1.45,1.,28.3990145788662));
#19663=CARTESIAN_POINT('',(-1.45,1.,28.5655857505187));
#19664=CARTESIAN_POINT('',(-1.45,-1.,28.3990145788662));
#19665=CARTESIAN_POINT('Origin',(-1.,-1.,28.2352279734464));
#19666=CARTESIAN_POINT('',(-1.,-1.,28.2352279734464));
#19667=CARTESIAN_POINT('',(-1.45,-1.,28.3990145788662));
#19668=CARTESIAN_POINT('',(-1.,1.,28.2352279734464));
#19669=CARTESIAN_POINT('',(-1.45,1.,28.3990145788662));
#19670=CARTESIAN_POINT('',(-1.,-1.,28.2352279734464));
#19671=CARTESIAN_POINT('Origin',(-1.,-1.,28.1010538252205));
#19672=CARTESIAN_POINT('',(-1.,-1.,28.1010538252205));
#19673=CARTESIAN_POINT('',(-1.,-1.,28.2352279734464));
#19674=CARTESIAN_POINT('',(-1.,1.,28.1010538252205));
#19675=CARTESIAN_POINT('',(-1.,1.,28.2352279734464));
#19676=CARTESIAN_POINT('',(-1.,-1.,28.1010538252205));
#19677=CARTESIAN_POINT('Origin',(-1.45,-1.,27.9372672198007));
#19678=CARTESIAN_POINT('',(-1.45,-1.,27.9372672198007));
#19679=CARTESIAN_POINT('',(-1.,-1.,28.1010538252205));
#19680=CARTESIAN_POINT('',(-1.45,1.,27.9372672198007));
#19681=CARTESIAN_POINT('',(-1.,1.,28.1010538252205));
#19682=CARTESIAN_POINT('',(-1.45,-1.,27.9372672198007));
#19683=CARTESIAN_POINT('Origin',(-1.45,-1.,27.7706960481482));
#19684=CARTESIAN_POINT('',(-1.45,-1.,27.7706960481482));
#19685=CARTESIAN_POINT('',(-1.45,-1.,27.9372672198007));
#19686=CARTESIAN_POINT('',(-1.45,1.,27.7706960481482));
#19687=CARTESIAN_POINT('',(-1.45,1.,27.9372672198007));
#19688=CARTESIAN_POINT('',(-1.45,-1.,27.7706960481482));
#19689=CARTESIAN_POINT('Origin',(-1.,-1.,27.6069094427284));
#19690=CARTESIAN_POINT('',(-1.,-1.,27.6069094427284));
#19691=CARTESIAN_POINT('',(-1.45,-1.,27.7706960481482));
#19692=CARTESIAN_POINT('',(-1.,1.,27.6069094427284));
#19693=CARTESIAN_POINT('',(-1.45,1.,27.7706960481482));
#19694=CARTESIAN_POINT('',(-1.,-1.,27.6069094427284));
#19695=CARTESIAN_POINT('Origin',(-1.,-1.,27.4727352945026));
#19696=CARTESIAN_POINT('',(-1.,-1.,27.4727352945026));
#19697=CARTESIAN_POINT('',(-1.,-1.,27.6069094427284));
#19698=CARTESIAN_POINT('',(-1.,1.,27.4727352945026));
#19699=CARTESIAN_POINT('',(-1.,1.,27.6069094427284));
#19700=CARTESIAN_POINT('',(-1.,-1.,27.4727352945026));
#19701=CARTESIAN_POINT('Origin',(-1.45,-1.,27.3089486890828));
#19702=CARTESIAN_POINT('',(-1.45,-1.,27.3089486890828));
#19703=CARTESIAN_POINT('',(-1.,-1.,27.4727352945026));
#19704=CARTESIAN_POINT('',(-1.45,1.,27.3089486890828));
#19705=CARTESIAN_POINT('',(-1.,1.,27.4727352945026));
#19706=CARTESIAN_POINT('',(-1.45,-1.,27.3089486890828));
#19707=CARTESIAN_POINT('Origin',(-1.45,-1.,27.1423775174303));
#19708=CARTESIAN_POINT('',(-1.45,-1.,27.1423775174303));
#19709=CARTESIAN_POINT('',(-1.45,-1.,27.3089486890828));
#19710=CARTESIAN_POINT('',(-1.45,1.,27.1423775174303));
#19711=CARTESIAN_POINT('',(-1.45,1.,27.3089486890828));
#19712=CARTESIAN_POINT('',(-1.45,-1.,27.1423775174303));
#19713=CARTESIAN_POINT('Origin',(-1.,-1.,26.9785909120105));
#19714=CARTESIAN_POINT('',(-1.,-1.,26.9785909120105));
#19715=CARTESIAN_POINT('',(-1.45,-1.,27.1423775174303));
#19716=CARTESIAN_POINT('',(-1.,1.,26.9785909120105));
#19717=CARTESIAN_POINT('',(-1.45,1.,27.1423775174303));
#19718=CARTESIAN_POINT('',(-1.,-1.,26.9785909120105));
#19719=CARTESIAN_POINT('Origin',(-1.,-1.,26.8444167637846));
#19720=CARTESIAN_POINT('',(-1.,-1.,26.8444167637846));
#19721=CARTESIAN_POINT('',(-1.,-1.,26.9785909120105));
#19722=CARTESIAN_POINT('',(-1.,1.,26.8444167637846));
#19723=CARTESIAN_POINT('',(-1.,1.,26.9785909120105));
#19724=CARTESIAN_POINT('',(-1.,-1.,26.8444167637846));
#19725=CARTESIAN_POINT('Origin',(-1.45,-1.,26.6806301583648));
#19726=CARTESIAN_POINT('',(-1.45,-1.,26.6806301583648));
#19727=CARTESIAN_POINT('',(-1.,-1.,26.8444167637846));
#19728=CARTESIAN_POINT('',(-1.45,1.,26.6806301583648));
#19729=CARTESIAN_POINT('',(-1.,1.,26.8444167637846));
#19730=CARTESIAN_POINT('',(-1.45,-1.,26.6806301583648));
#19731=CARTESIAN_POINT('Origin',(-1.45,-1.,26.5140589867123));
#19732=CARTESIAN_POINT('',(-1.45,-1.,26.5140589867123));
#19733=CARTESIAN_POINT('',(-1.45,-1.,26.6806301583648));
#19734=CARTESIAN_POINT('',(-1.45,1.,26.5140589867123));
#19735=CARTESIAN_POINT('',(-1.45,1.,26.6806301583648));
#19736=CARTESIAN_POINT('',(-1.45,-1.,26.5140589867123));
#19737=CARTESIAN_POINT('Origin',(-1.,-1.,26.3502723812925));
#19738=CARTESIAN_POINT('',(-1.,-1.,26.3502723812925));
#19739=CARTESIAN_POINT('',(-1.45,-1.,26.5140589867123));
#19740=CARTESIAN_POINT('',(-1.,1.,26.3502723812925));
#19741=CARTESIAN_POINT('',(-1.45,1.,26.5140589867123));
#19742=CARTESIAN_POINT('',(-1.,-1.,26.3502723812925));
#19743=CARTESIAN_POINT('Origin',(-1.,-1.,26.2160982330666));
#19744=CARTESIAN_POINT('',(-1.,-1.,26.2160982330666));
#19745=CARTESIAN_POINT('',(-1.,-1.,26.3502723812925));
#19746=CARTESIAN_POINT('',(-1.,1.,26.2160982330666));
#19747=CARTESIAN_POINT('',(-1.,1.,26.3502723812925));
#19748=CARTESIAN_POINT('',(-1.,-1.,26.2160982330666));
#19749=CARTESIAN_POINT('Origin',(-1.45,-1.,26.0523116276469));
#19750=CARTESIAN_POINT('',(-1.45,-1.,26.0523116276469));
#19751=CARTESIAN_POINT('',(-1.,-1.,26.2160982330666));
#19752=CARTESIAN_POINT('',(-1.45,1.,26.0523116276469));
#19753=CARTESIAN_POINT('',(-1.,1.,26.2160982330666));
#19754=CARTESIAN_POINT('',(-1.45,-1.,26.0523116276469));
#19755=CARTESIAN_POINT('Origin',(-1.45,-1.,25.8857404559944));
#19756=CARTESIAN_POINT('',(-1.45,-1.,25.8857404559944));
#19757=CARTESIAN_POINT('',(-1.45,-1.,26.0523116276469));
#19758=CARTESIAN_POINT('',(-1.45,1.,25.8857404559944));
#19759=CARTESIAN_POINT('',(-1.45,1.,26.0523116276469));
#19760=CARTESIAN_POINT('',(-1.45,-1.,25.8857404559944));
#19761=CARTESIAN_POINT('Origin',(-1.,-1.,25.7219538505746));
#19762=CARTESIAN_POINT('',(-1.,-1.,25.7219538505746));
#19763=CARTESIAN_POINT('',(-1.45,-1.,25.8857404559944));
#19764=CARTESIAN_POINT('',(-1.,1.,25.7219538505746));
#19765=CARTESIAN_POINT('',(-1.45,1.,25.8857404559944));
#19766=CARTESIAN_POINT('',(-1.,-1.,25.7219538505746));
#19767=CARTESIAN_POINT('Origin',(-1.,-1.,25.5877797023487));
#19768=CARTESIAN_POINT('',(-1.,-1.,25.5877797023487));
#19769=CARTESIAN_POINT('',(-1.,-1.,25.7219538505746));
#19770=CARTESIAN_POINT('',(-1.,1.,25.5877797023487));
#19771=CARTESIAN_POINT('',(-1.,1.,25.7219538505746));
#19772=CARTESIAN_POINT('',(-1.,-1.,25.5877797023487));
#19773=CARTESIAN_POINT('Origin',(-1.45,-1.,25.4239930969289));
#19774=CARTESIAN_POINT('',(-1.45,-1.,25.4239930969289));
#19775=CARTESIAN_POINT('',(-1.,-1.,25.5877797023487));
#19776=CARTESIAN_POINT('',(-1.45,1.,25.4239930969289));
#19777=CARTESIAN_POINT('',(-1.,1.,25.5877797023487));
#19778=CARTESIAN_POINT('',(-1.45,-1.,25.4239930969289));
#19779=CARTESIAN_POINT('Origin',(-1.45,-1.,25.2574219252764));
#19780=CARTESIAN_POINT('',(-1.45,-1.,25.2574219252764));
#19781=CARTESIAN_POINT('',(-1.45,-1.,25.4239930969289));
#19782=CARTESIAN_POINT('',(-1.45,1.,25.2574219252764));
#19783=CARTESIAN_POINT('',(-1.45,1.,25.4239930969289));
#19784=CARTESIAN_POINT('',(-1.45,-1.,25.2574219252764));
#19785=CARTESIAN_POINT('Origin',(-1.,-1.,25.0936353198566));
#19786=CARTESIAN_POINT('',(-1.,-1.,25.0936353198566));
#19787=CARTESIAN_POINT('',(-1.45,-1.,25.2574219252764));
#19788=CARTESIAN_POINT('',(-1.,1.,25.0936353198566));
#19789=CARTESIAN_POINT('',(-1.45,1.,25.2574219252764));
#19790=CARTESIAN_POINT('',(-1.,-1.,25.0936353198566));
#19791=CARTESIAN_POINT('Origin',(-1.,-1.,24.9594611716307));
#19792=CARTESIAN_POINT('',(-1.,-1.,24.9594611716307));
#19793=CARTESIAN_POINT('',(-1.,-1.,25.0936353198566));
#19794=CARTESIAN_POINT('',(-1.,1.,24.9594611716307));
#19795=CARTESIAN_POINT('',(-1.,1.,25.0936353198566));
#19796=CARTESIAN_POINT('',(-1.,-1.,24.9594611716307));
#19797=CARTESIAN_POINT('Origin',(-1.45,-1.,24.7956745662109));
#19798=CARTESIAN_POINT('',(-1.45,-1.,24.7956745662109));
#19799=CARTESIAN_POINT('',(-1.,-1.,24.9594611716307));
#19800=CARTESIAN_POINT('',(-1.45,1.,24.7956745662109));
#19801=CARTESIAN_POINT('',(-1.,1.,24.9594611716307));
#19802=CARTESIAN_POINT('',(-1.45,-1.,24.7956745662109));
#19803=CARTESIAN_POINT('Origin',(-1.45,-1.,24.6291033945584));
#19804=CARTESIAN_POINT('',(-1.45,-1.,24.6291033945584));
#19805=CARTESIAN_POINT('',(-1.45,-1.,24.7956745662109));
#19806=CARTESIAN_POINT('',(-1.45,1.,24.6291033945584));
#19807=CARTESIAN_POINT('',(-1.45,1.,24.7956745662109));
#19808=CARTESIAN_POINT('',(-1.45,-1.,24.6291033945584));
#19809=CARTESIAN_POINT('Origin',(-1.,-1.,24.4653167891386));
#19810=CARTESIAN_POINT('',(-1.,-1.,24.4653167891386));
#19811=CARTESIAN_POINT('',(-1.45,-1.,24.6291033945584));
#19812=CARTESIAN_POINT('',(-1.,1.,24.4653167891386));
#19813=CARTESIAN_POINT('',(-1.45,1.,24.6291033945584));
#19814=CARTESIAN_POINT('',(-1.,-1.,24.4653167891386));
#19815=CARTESIAN_POINT('Origin',(-1.,-1.,24.3311426409128));
#19816=CARTESIAN_POINT('',(-1.,-1.,24.3311426409128));
#19817=CARTESIAN_POINT('',(-1.,-1.,24.4653167891386));
#19818=CARTESIAN_POINT('',(-1.,1.,24.3311426409128));
#19819=CARTESIAN_POINT('',(-1.,1.,24.4653167891386));
#19820=CARTESIAN_POINT('',(-1.,-1.,24.3311426409128));
#19821=CARTESIAN_POINT('Origin',(-1.45,-1.,24.167356035493));
#19822=CARTESIAN_POINT('',(-1.45,-1.,24.167356035493));
#19823=CARTESIAN_POINT('',(-1.,-1.,24.3311426409128));
#19824=CARTESIAN_POINT('',(-1.45,1.,24.167356035493));
#19825=CARTESIAN_POINT('',(-1.,1.,24.3311426409128));
#19826=CARTESIAN_POINT('',(-1.45,-1.,24.167356035493));
#19827=CARTESIAN_POINT('Origin',(-1.45,-1.,24.0007848638405));
#19828=CARTESIAN_POINT('',(-1.45,-1.,24.0007848638405));
#19829=CARTESIAN_POINT('',(-1.45,-1.,24.167356035493));
#19830=CARTESIAN_POINT('',(-1.45,1.,24.0007848638405));
#19831=CARTESIAN_POINT('',(-1.45,1.,24.167356035493));
#19832=CARTESIAN_POINT('',(-1.45,-1.,24.0007848638405));
#19833=CARTESIAN_POINT('Origin',(-1.,-1.,23.8369982584207));
#19834=CARTESIAN_POINT('',(-1.,-1.,23.8369982584207));
#19835=CARTESIAN_POINT('',(-1.45,-1.,24.0007848638405));
#19836=CARTESIAN_POINT('',(-1.,1.,23.8369982584207));
#19837=CARTESIAN_POINT('',(-1.45,1.,24.0007848638405));
#19838=CARTESIAN_POINT('',(-1.,-1.,23.8369982584207));
#19839=CARTESIAN_POINT('Origin',(-1.,-1.,23.7028241101948));
#19840=CARTESIAN_POINT('',(-1.,-1.,23.7028241101948));
#19841=CARTESIAN_POINT('',(-1.,-1.,23.8369982584207));
#19842=CARTESIAN_POINT('',(-1.,1.,23.7028241101948));
#19843=CARTESIAN_POINT('',(-1.,1.,23.8369982584207));
#19844=CARTESIAN_POINT('',(-1.,-1.,23.7028241101948));
#19845=CARTESIAN_POINT('Origin',(-1.45,-1.,23.539037504775));
#19846=CARTESIAN_POINT('',(-1.45,-1.,23.539037504775));
#19847=CARTESIAN_POINT('',(-1.,-1.,23.7028241101948));
#19848=CARTESIAN_POINT('',(-1.45,1.,23.539037504775));
#19849=CARTESIAN_POINT('',(-1.,1.,23.7028241101948));
#19850=CARTESIAN_POINT('',(-1.45,-1.,23.539037504775));
#19851=CARTESIAN_POINT('Origin',(-1.45,-1.,23.3724663331225));
#19852=CARTESIAN_POINT('',(-1.45,-1.,23.3724663331225));
#19853=CARTESIAN_POINT('',(-1.45,-1.,23.539037504775));
#19854=CARTESIAN_POINT('',(-1.45,1.,23.3724663331225));
#19855=CARTESIAN_POINT('',(-1.45,1.,23.539037504775));
#19856=CARTESIAN_POINT('',(-1.45,-1.,23.3724663331225));
#19857=CARTESIAN_POINT('Origin',(-1.,-1.,23.2086797277027));
#19858=CARTESIAN_POINT('',(-1.,-1.,23.2086797277027));
#19859=CARTESIAN_POINT('',(-1.45,-1.,23.3724663331225));
#19860=CARTESIAN_POINT('',(-1.,1.,23.2086797277027));
#19861=CARTESIAN_POINT('',(-1.45,1.,23.3724663331225));
#19862=CARTESIAN_POINT('',(-1.,-1.,23.2086797277027));
#19863=CARTESIAN_POINT('Origin',(-1.,-1.,23.0745055794769));
#19864=CARTESIAN_POINT('',(-1.,-1.,23.0745055794769));
#19865=CARTESIAN_POINT('',(-1.,-1.,23.2086797277027));
#19866=CARTESIAN_POINT('',(-1.,1.,23.0745055794769));
#19867=CARTESIAN_POINT('',(-1.,1.,23.2086797277027));
#19868=CARTESIAN_POINT('',(-1.,-1.,23.0745055794769));
#19869=CARTESIAN_POINT('Origin',(-1.45,-1.,22.9107189740571));
#19870=CARTESIAN_POINT('',(-1.45,-1.,22.9107189740571));
#19871=CARTESIAN_POINT('',(-1.,-1.,23.0745055794769));
#19872=CARTESIAN_POINT('',(-1.45,1.,22.9107189740571));
#19873=CARTESIAN_POINT('',(-1.,1.,23.0745055794769));
#19874=CARTESIAN_POINT('',(-1.45,-1.,22.9107189740571));
#19875=CARTESIAN_POINT('Origin',(-1.45,-1.,22.7441478024046));
#19876=CARTESIAN_POINT('',(-1.45,-1.,22.7441478024046));
#19877=CARTESIAN_POINT('',(-1.45,-1.,22.9107189740571));
#19878=CARTESIAN_POINT('',(-1.45,1.,22.7441478024046));
#19879=CARTESIAN_POINT('',(-1.45,1.,22.9107189740571));
#19880=CARTESIAN_POINT('',(-1.45,-1.,22.7441478024046));
#19881=CARTESIAN_POINT('Origin',(-1.,-1.,22.5803611969848));
#19882=CARTESIAN_POINT('',(-1.,-1.,22.5803611969848));
#19883=CARTESIAN_POINT('',(-1.45,-1.,22.7441478024046));
#19884=CARTESIAN_POINT('',(-1.,1.,22.5803611969848));
#19885=CARTESIAN_POINT('',(-1.45,1.,22.7441478024046));
#19886=CARTESIAN_POINT('',(-1.,-1.,22.5803611969848));
#19887=CARTESIAN_POINT('Origin',(-1.,-1.,22.4461870487589));
#19888=CARTESIAN_POINT('',(-1.,-1.,22.4461870487589));
#19889=CARTESIAN_POINT('',(-1.,-1.,22.5803611969848));
#19890=CARTESIAN_POINT('',(-1.,1.,22.4461870487589));
#19891=CARTESIAN_POINT('',(-1.,1.,22.5803611969848));
#19892=CARTESIAN_POINT('',(-1.,-1.,22.4461870487589));
#19893=CARTESIAN_POINT('Origin',(-1.45,-1.,22.2824004433391));
#19894=CARTESIAN_POINT('',(-1.45,-1.,22.2824004433391));
#19895=CARTESIAN_POINT('',(-1.,-1.,22.4461870487589));
#19896=CARTESIAN_POINT('',(-1.45,1.,22.2824004433391));
#19897=CARTESIAN_POINT('',(-1.,1.,22.4461870487589));
#19898=CARTESIAN_POINT('',(-1.45,-1.,22.2824004433391));
#19899=CARTESIAN_POINT('Origin',(-1.45,-1.,22.1158292716866));
#19900=CARTESIAN_POINT('',(-1.45,-1.,22.1158292716866));
#19901=CARTESIAN_POINT('',(-1.45,-1.,22.2824004433391));
#19902=CARTESIAN_POINT('',(-1.45,1.,22.1158292716866));
#19903=CARTESIAN_POINT('',(-1.45,1.,22.2824004433391));
#19904=CARTESIAN_POINT('',(-1.45,-1.,22.1158292716866));
#19905=CARTESIAN_POINT('Origin',(-1.,-1.,21.9520426662668));
#19906=CARTESIAN_POINT('',(-1.,-1.,21.9520426662668));
#19907=CARTESIAN_POINT('',(-1.45,-1.,22.1158292716866));
#19908=CARTESIAN_POINT('',(-1.,1.,21.9520426662668));
#19909=CARTESIAN_POINT('',(-1.45,1.,22.1158292716866));
#19910=CARTESIAN_POINT('',(-1.,-1.,21.9520426662668));
#19911=CARTESIAN_POINT('Origin',(-1.,-1.,21.8178685180409));
#19912=CARTESIAN_POINT('',(-1.,-1.,21.8178685180409));
#19913=CARTESIAN_POINT('',(-1.,-1.,21.9520426662668));
#19914=CARTESIAN_POINT('',(-1.,1.,21.8178685180409));
#19915=CARTESIAN_POINT('',(-1.,1.,21.9520426662668));
#19916=CARTESIAN_POINT('',(-1.,-1.,21.8178685180409));
#19917=CARTESIAN_POINT('Origin',(-1.45,-1.,21.6540819126211));
#19918=CARTESIAN_POINT('',(-1.45,-1.,21.6540819126211));
#19919=CARTESIAN_POINT('',(-1.,-1.,21.8178685180409));
#19920=CARTESIAN_POINT('',(-1.45,1.,21.6540819126211));
#19921=CARTESIAN_POINT('',(-1.,1.,21.8178685180409));
#19922=CARTESIAN_POINT('',(-1.45,-1.,21.6540819126211));
#19923=CARTESIAN_POINT('Origin',(-1.45,-1.,21.4875107409686));
#19924=CARTESIAN_POINT('',(-1.45,-1.,21.4875107409686));
#19925=CARTESIAN_POINT('',(-1.45,-1.,21.6540819126211));
#19926=CARTESIAN_POINT('',(-1.45,1.,21.4875107409686));
#19927=CARTESIAN_POINT('',(-1.45,1.,21.6540819126211));
#19928=CARTESIAN_POINT('',(-1.45,-1.,21.4875107409686));
#19929=CARTESIAN_POINT('Origin',(-1.,-1.,21.3237241355489));
#19930=CARTESIAN_POINT('',(-1.,-1.,21.3237241355489));
#19931=CARTESIAN_POINT('',(-1.45,-1.,21.4875107409686));
#19932=CARTESIAN_POINT('',(-1.,1.,21.3237241355489));
#19933=CARTESIAN_POINT('',(-1.45,1.,21.4875107409686));
#19934=CARTESIAN_POINT('',(-1.,-1.,21.3237241355489));
#19935=CARTESIAN_POINT('Origin',(-1.,-1.,21.189549987323));
#19936=CARTESIAN_POINT('',(-1.,-1.,21.189549987323));
#19937=CARTESIAN_POINT('',(-1.,-1.,21.3237241355489));
#19938=CARTESIAN_POINT('',(-1.,1.,21.189549987323));
#19939=CARTESIAN_POINT('',(-1.,1.,21.3237241355489));
#19940=CARTESIAN_POINT('',(-1.,-1.,21.189549987323));
#19941=CARTESIAN_POINT('Origin',(-1.45,-1.,21.0257633819032));
#19942=CARTESIAN_POINT('',(-1.45,-1.,21.0257633819032));
#19943=CARTESIAN_POINT('',(-1.,-1.,21.189549987323));
#19944=CARTESIAN_POINT('',(-1.45,1.,21.0257633819032));
#19945=CARTESIAN_POINT('',(-1.,1.,21.189549987323));
#19946=CARTESIAN_POINT('',(-1.45,-1.,21.0257633819032));
#19947=CARTESIAN_POINT('Origin',(-1.45,-1.,20.8591922102507));
#19948=CARTESIAN_POINT('',(-1.45,-1.,20.8591922102507));
#19949=CARTESIAN_POINT('',(-1.45,-1.,21.0257633819032));
#19950=CARTESIAN_POINT('',(-1.45,1.,20.8591922102507));
#19951=CARTESIAN_POINT('',(-1.45,1.,21.0257633819032));
#19952=CARTESIAN_POINT('',(-1.45,-1.,20.8591922102507));
#19953=CARTESIAN_POINT('Origin',(-1.,-1.,20.6954056048309));
#19954=CARTESIAN_POINT('',(-1.,-1.,20.6954056048309));
#19955=CARTESIAN_POINT('',(-1.45,-1.,20.8591922102507));
#19956=CARTESIAN_POINT('',(-1.,1.,20.6954056048309));
#19957=CARTESIAN_POINT('',(-1.45,1.,20.8591922102507));
#19958=CARTESIAN_POINT('',(-1.,-1.,20.6954056048309));
#19959=CARTESIAN_POINT('Origin',(-1.,-1.,20.561231456605));
#19960=CARTESIAN_POINT('',(-1.,-1.,20.561231456605));
#19961=CARTESIAN_POINT('',(-1.,-1.,20.6954056048309));
#19962=CARTESIAN_POINT('',(-1.,1.,20.561231456605));
#19963=CARTESIAN_POINT('',(-1.,1.,20.6954056048309));
#19964=CARTESIAN_POINT('',(-1.,-1.,20.561231456605));
#19965=CARTESIAN_POINT('Origin',(-1.45,-1.,20.3974448511852));
#19966=CARTESIAN_POINT('',(-1.45,-1.,20.3974448511852));
#19967=CARTESIAN_POINT('',(-1.,-1.,20.561231456605));
#19968=CARTESIAN_POINT('',(-1.45,1.,20.3974448511852));
#19969=CARTESIAN_POINT('',(-1.,1.,20.561231456605));
#19970=CARTESIAN_POINT('',(-1.45,-1.,20.3974448511852));
#19971=CARTESIAN_POINT('Origin',(-1.45,-1.,20.2308736795327));
#19972=CARTESIAN_POINT('',(-1.45,-1.,20.2308736795327));
#19973=CARTESIAN_POINT('',(-1.45,-1.,20.3974448511852));
#19974=CARTESIAN_POINT('',(-1.45,1.,20.2308736795327));
#19975=CARTESIAN_POINT('',(-1.45,1.,20.3974448511852));
#19976=CARTESIAN_POINT('',(-1.45,-1.,20.2308736795327));
#19977=CARTESIAN_POINT('Origin',(-1.,-1.,20.0670870741129));
#19978=CARTESIAN_POINT('',(-1.,-1.,20.0670870741129));
#19979=CARTESIAN_POINT('',(-1.45,-1.,20.2308736795327));
#19980=CARTESIAN_POINT('',(-1.,1.,20.0670870741129));
#19981=CARTESIAN_POINT('',(-1.45,1.,20.2308736795327));
#19982=CARTESIAN_POINT('',(-1.,-1.,20.0670870741129));
#19983=CARTESIAN_POINT('Origin',(-1.,-1.,19.9329129258871));
#19984=CARTESIAN_POINT('',(-1.,-1.,19.9329129258871));
#19985=CARTESIAN_POINT('',(-1.,-1.,20.0670870741129));
#19986=CARTESIAN_POINT('',(-1.,1.,19.9329129258871));
#19987=CARTESIAN_POINT('',(-1.,1.,20.0670870741129));
#19988=CARTESIAN_POINT('',(-1.,-1.,19.9329129258871));
#19989=CARTESIAN_POINT('Origin',(-1.45,-1.,19.7691263204673));
#19990=CARTESIAN_POINT('',(-1.45,-1.,19.7691263204673));
#19991=CARTESIAN_POINT('',(-1.,-1.,19.9329129258871));
#19992=CARTESIAN_POINT('',(-1.45,1.,19.7691263204673));
#19993=CARTESIAN_POINT('',(-1.,1.,19.9329129258871));
#19994=CARTESIAN_POINT('',(-1.45,-1.,19.7691263204673));
#19995=CARTESIAN_POINT('Origin',(-1.45,-1.,19.6025551488148));
#19996=CARTESIAN_POINT('',(-1.45,-1.,19.6025551488148));
#19997=CARTESIAN_POINT('',(-1.45,-1.,19.7691263204673));
#19998=CARTESIAN_POINT('',(-1.45,1.,19.6025551488148));
#19999=CARTESIAN_POINT('',(-1.45,1.,19.7691263204673));
#20000=CARTESIAN_POINT('',(-1.45,-1.,19.6025551488148));
#20001=CARTESIAN_POINT('Origin',(-1.,-1.,19.438768543395));
#20002=CARTESIAN_POINT('',(-1.,-1.,19.438768543395));
#20003=CARTESIAN_POINT('',(-1.45,-1.,19.6025551488148));
#20004=CARTESIAN_POINT('',(-1.,1.,19.438768543395));
#20005=CARTESIAN_POINT('',(-1.45,1.,19.6025551488148));
#20006=CARTESIAN_POINT('',(-1.,-1.,19.438768543395));
#20007=CARTESIAN_POINT('Origin',(-1.,-1.,19.3045943951691));
#20008=CARTESIAN_POINT('',(-1.,-1.,19.3045943951691));
#20009=CARTESIAN_POINT('',(-1.,-1.,19.438768543395));
#20010=CARTESIAN_POINT('',(-1.,1.,19.3045943951691));
#20011=CARTESIAN_POINT('',(-1.,1.,19.438768543395));
#20012=CARTESIAN_POINT('',(-1.,-1.,19.3045943951691));
#20013=CARTESIAN_POINT('Origin',(-1.45,-1.,19.1408077897493));
#20014=CARTESIAN_POINT('',(-1.45,-1.,19.1408077897493));
#20015=CARTESIAN_POINT('',(-1.,-1.,19.3045943951691));
#20016=CARTESIAN_POINT('',(-1.45,1.,19.1408077897493));
#20017=CARTESIAN_POINT('',(-1.,1.,19.3045943951691));
#20018=CARTESIAN_POINT('',(-1.45,-1.,19.1408077897493));
#20019=CARTESIAN_POINT('Origin',(-1.45,-1.,18.9742366180968));
#20020=CARTESIAN_POINT('',(-1.45,-1.,18.9742366180968));
#20021=CARTESIAN_POINT('',(-1.45,-1.,19.1408077897493));
#20022=CARTESIAN_POINT('',(-1.45,1.,18.9742366180968));
#20023=CARTESIAN_POINT('',(-1.45,1.,19.1408077897493));
#20024=CARTESIAN_POINT('',(-1.45,-1.,18.9742366180968));
#20025=CARTESIAN_POINT('Origin',(-1.,-1.,18.810450012677));
#20026=CARTESIAN_POINT('',(-1.,-1.,18.810450012677));
#20027=CARTESIAN_POINT('',(-1.45,-1.,18.9742366180968));
#20028=CARTESIAN_POINT('',(-1.,1.,18.810450012677));
#20029=CARTESIAN_POINT('',(-1.45,1.,18.9742366180968));
#20030=CARTESIAN_POINT('',(-1.,-1.,18.810450012677));
#20031=CARTESIAN_POINT('Origin',(-1.,-1.,18.6762758644511));
#20032=CARTESIAN_POINT('',(-1.,-1.,18.6762758644511));
#20033=CARTESIAN_POINT('',(-1.,-1.,18.810450012677));
#20034=CARTESIAN_POINT('',(-1.,1.,18.6762758644511));
#20035=CARTESIAN_POINT('',(-1.,1.,18.810450012677));
#20036=CARTESIAN_POINT('',(-1.,-1.,18.6762758644511));
#20037=CARTESIAN_POINT('Origin',(-1.45,-1.,18.5124892590314));
#20038=CARTESIAN_POINT('',(-1.45,-1.,18.5124892590314));
#20039=CARTESIAN_POINT('',(-1.,-1.,18.6762758644511));
#20040=CARTESIAN_POINT('',(-1.45,1.,18.5124892590314));
#20041=CARTESIAN_POINT('',(-1.,1.,18.6762758644511));
#20042=CARTESIAN_POINT('',(-1.45,-1.,18.5124892590314));
#20043=CARTESIAN_POINT('Origin',(-1.45,-1.,18.3459180873789));
#20044=CARTESIAN_POINT('',(-1.45,-1.,18.3459180873789));
#20045=CARTESIAN_POINT('',(-1.45,-1.,18.5124892590314));
#20046=CARTESIAN_POINT('',(-1.45,1.,18.3459180873789));
#20047=CARTESIAN_POINT('',(-1.45,1.,18.5124892590314));
#20048=CARTESIAN_POINT('',(-1.45,-1.,18.3459180873789));
#20049=CARTESIAN_POINT('Origin',(-1.,-1.,18.1821314819591));
#20050=CARTESIAN_POINT('',(-1.,-1.,18.1821314819591));
#20051=CARTESIAN_POINT('',(-1.45,-1.,18.3459180873789));
#20052=CARTESIAN_POINT('',(-1.,1.,18.1821314819591));
#20053=CARTESIAN_POINT('',(-1.45,1.,18.3459180873789));
#20054=CARTESIAN_POINT('',(-1.,-1.,18.1821314819591));
#20055=CARTESIAN_POINT('Origin',(-1.,-1.,18.0479573337332));
#20056=CARTESIAN_POINT('',(-1.,-1.,18.0479573337332));
#20057=CARTESIAN_POINT('',(-1.,-1.,18.1821314819591));
#20058=CARTESIAN_POINT('',(-1.,1.,18.0479573337332));
#20059=CARTESIAN_POINT('',(-1.,1.,18.1821314819591));
#20060=CARTESIAN_POINT('',(-1.,-1.,18.0479573337332));
#20061=CARTESIAN_POINT('Origin',(-1.45,-1.,17.8841707283134));
#20062=CARTESIAN_POINT('',(-1.45,-1.,17.8841707283134));
#20063=CARTESIAN_POINT('',(-1.,-1.,18.0479573337332));
#20064=CARTESIAN_POINT('',(-1.45,1.,17.8841707283134));
#20065=CARTESIAN_POINT('',(-1.,1.,18.0479573337332));
#20066=CARTESIAN_POINT('',(-1.45,-1.,17.8841707283134));
#20067=CARTESIAN_POINT('Origin',(-1.45,-1.,17.7175995566609));
#20068=CARTESIAN_POINT('',(-1.45,-1.,17.7175995566609));
#20069=CARTESIAN_POINT('',(-1.45,-1.,17.8841707283134));
#20070=CARTESIAN_POINT('',(-1.45,1.,17.7175995566609));
#20071=CARTESIAN_POINT('',(-1.45,1.,17.8841707283134));
#20072=CARTESIAN_POINT('',(-1.45,-1.,17.7175995566609));
#20073=CARTESIAN_POINT('Origin',(-1.,-1.,17.5538129512411));
#20074=CARTESIAN_POINT('',(-1.,-1.,17.5538129512411));
#20075=CARTESIAN_POINT('',(-1.45,-1.,17.7175995566609));
#20076=CARTESIAN_POINT('',(-1.,1.,17.5538129512411));
#20077=CARTESIAN_POINT('',(-1.45,1.,17.7175995566609));
#20078=CARTESIAN_POINT('',(-1.,-1.,17.5538129512411));
#20079=CARTESIAN_POINT('Origin',(-1.,-1.,17.4196388030152));
#20080=CARTESIAN_POINT('',(-1.,-1.,17.4196388030152));
#20081=CARTESIAN_POINT('',(-1.,-1.,17.5538129512411));
#20082=CARTESIAN_POINT('',(-1.,1.,17.4196388030152));
#20083=CARTESIAN_POINT('',(-1.,1.,17.5538129512411));
#20084=CARTESIAN_POINT('',(-1.,-1.,17.4196388030152));
#20085=CARTESIAN_POINT('Origin',(-1.45,-1.,17.2558521975954));
#20086=CARTESIAN_POINT('',(-1.45,-1.,17.2558521975954));
#20087=CARTESIAN_POINT('',(-1.,-1.,17.4196388030152));
#20088=CARTESIAN_POINT('',(-1.45,1.,17.2558521975954));
#20089=CARTESIAN_POINT('',(-1.,1.,17.4196388030152));
#20090=CARTESIAN_POINT('',(-1.45,-1.,17.2558521975954));
#20091=CARTESIAN_POINT('Origin',(-1.45,-1.,17.0892810259429));
#20092=CARTESIAN_POINT('',(-1.45,-1.,17.0892810259429));
#20093=CARTESIAN_POINT('',(-1.45,-1.,17.2558521975954));
#20094=CARTESIAN_POINT('',(-1.45,1.,17.0892810259429));
#20095=CARTESIAN_POINT('',(-1.45,1.,17.2558521975954));
#20096=CARTESIAN_POINT('',(-1.45,-1.,17.0892810259429));
#20097=CARTESIAN_POINT('Origin',(-1.,-1.,16.9254944205231));
#20098=CARTESIAN_POINT('',(-1.,-1.,16.9254944205231));
#20099=CARTESIAN_POINT('',(-1.45,-1.,17.0892810259429));
#20100=CARTESIAN_POINT('',(-1.,1.,16.9254944205231));
#20101=CARTESIAN_POINT('',(-1.45,1.,17.0892810259429));
#20102=CARTESIAN_POINT('',(-1.,-1.,16.9254944205231));
#20103=CARTESIAN_POINT('Origin',(-1.,-1.,16.7913202722973));
#20104=CARTESIAN_POINT('',(-1.,-1.,16.7913202722973));
#20105=CARTESIAN_POINT('',(-1.,-1.,16.9254944205231));
#20106=CARTESIAN_POINT('',(-1.,1.,16.7913202722973));
#20107=CARTESIAN_POINT('',(-1.,1.,16.9254944205231));
#20108=CARTESIAN_POINT('',(-1.,-1.,16.7913202722973));
#20109=CARTESIAN_POINT('Origin',(-1.45,-1.,16.6275336668775));
#20110=CARTESIAN_POINT('',(-1.45,-1.,16.6275336668775));
#20111=CARTESIAN_POINT('',(-1.,-1.,16.7913202722973));
#20112=CARTESIAN_POINT('',(-1.45,1.,16.6275336668775));
#20113=CARTESIAN_POINT('',(-1.,1.,16.7913202722973));
#20114=CARTESIAN_POINT('',(-1.45,-1.,16.6275336668775));
#20115=CARTESIAN_POINT('Origin',(-1.45,-1.,16.460962495225));
#20116=CARTESIAN_POINT('',(-1.45,-1.,16.460962495225));
#20117=CARTESIAN_POINT('',(-1.45,-1.,16.6275336668775));
#20118=CARTESIAN_POINT('',(-1.45,1.,16.460962495225));
#20119=CARTESIAN_POINT('',(-1.45,1.,16.6275336668775));
#20120=CARTESIAN_POINT('',(-1.45,-1.,16.460962495225));
#20121=CARTESIAN_POINT('Origin',(-1.,-1.,16.2971758898052));
#20122=CARTESIAN_POINT('',(-1.,-1.,16.2971758898052));
#20123=CARTESIAN_POINT('',(-1.45,-1.,16.460962495225));
#20124=CARTESIAN_POINT('',(-1.,1.,16.2971758898052));
#20125=CARTESIAN_POINT('',(-1.45,1.,16.460962495225));
#20126=CARTESIAN_POINT('',(-1.,-1.,16.2971758898052));
#20127=CARTESIAN_POINT('Origin',(-1.,-1.,16.1630017415793));
#20128=CARTESIAN_POINT('',(-1.,-1.,16.1630017415793));
#20129=CARTESIAN_POINT('',(-1.,-1.,16.2971758898052));
#20130=CARTESIAN_POINT('',(-1.,1.,16.1630017415793));
#20131=CARTESIAN_POINT('',(-1.,1.,16.2971758898052));
#20132=CARTESIAN_POINT('',(-1.,-1.,16.1630017415793));
#20133=CARTESIAN_POINT('Origin',(-1.45,-1.,15.9992151361595));
#20134=CARTESIAN_POINT('',(-1.45,-1.,15.9992151361595));
#20135=CARTESIAN_POINT('',(-1.,-1.,16.1630017415793));
#20136=CARTESIAN_POINT('',(-1.45,1.,15.9992151361595));
#20137=CARTESIAN_POINT('',(-1.,1.,16.1630017415793));
#20138=CARTESIAN_POINT('',(-1.45,-1.,15.9992151361595));
#20139=CARTESIAN_POINT('Origin',(-1.45,-1.,15.832643964507));
#20140=CARTESIAN_POINT('',(-1.45,-1.,15.832643964507));
#20141=CARTESIAN_POINT('',(-1.45,-1.,15.9992151361595));
#20142=CARTESIAN_POINT('',(-1.45,1.,15.832643964507));
#20143=CARTESIAN_POINT('',(-1.45,1.,15.9992151361595));
#20144=CARTESIAN_POINT('',(-1.45,-1.,15.832643964507));
#20145=CARTESIAN_POINT('Origin',(-1.,-1.,15.6688573590872));
#20146=CARTESIAN_POINT('',(-1.,-1.,15.6688573590872));
#20147=CARTESIAN_POINT('',(-1.45,-1.,15.832643964507));
#20148=CARTESIAN_POINT('',(-1.,1.,15.6688573590872));
#20149=CARTESIAN_POINT('',(-1.45,1.,15.832643964507));
#20150=CARTESIAN_POINT('',(-1.,-1.,15.6688573590872));
#20151=CARTESIAN_POINT('Origin',(-1.,-1.,15.5346832108613));
#20152=CARTESIAN_POINT('',(-1.,-1.,15.5346832108613));
#20153=CARTESIAN_POINT('',(-1.,-1.,15.6688573590872));
#20154=CARTESIAN_POINT('',(-1.,1.,15.5346832108613));
#20155=CARTESIAN_POINT('',(-1.,1.,15.6688573590872));
#20156=CARTESIAN_POINT('',(-1.,-1.,15.5346832108613));
#20157=CARTESIAN_POINT('Origin',(-1.45,-1.,15.3708966054416));
#20158=CARTESIAN_POINT('',(-1.45,-1.,15.3708966054416));
#20159=CARTESIAN_POINT('',(-1.,-1.,15.5346832108613));
#20160=CARTESIAN_POINT('',(-1.45,1.,15.3708966054416));
#20161=CARTESIAN_POINT('',(-1.,1.,15.5346832108613));
#20162=CARTESIAN_POINT('',(-1.45,-1.,15.3708966054416));
#20163=CARTESIAN_POINT('Origin',(-1.45,-1.,15.2043254337891));
#20164=CARTESIAN_POINT('',(-1.45,-1.,15.2043254337891));
#20165=CARTESIAN_POINT('',(-1.45,-1.,15.3708966054416));
#20166=CARTESIAN_POINT('',(-1.45,1.,15.2043254337891));
#20167=CARTESIAN_POINT('',(-1.45,1.,15.3708966054416));
#20168=CARTESIAN_POINT('',(-1.45,-1.,15.2043254337891));
#20169=CARTESIAN_POINT('Origin',(-1.,-1.,15.0405388283693));
#20170=CARTESIAN_POINT('',(-1.,-1.,15.0405388283693));
#20171=CARTESIAN_POINT('',(-1.45,-1.,15.2043254337891));
#20172=CARTESIAN_POINT('',(-1.,1.,15.0405388283693));
#20173=CARTESIAN_POINT('',(-1.45,1.,15.2043254337891));
#20174=CARTESIAN_POINT('',(-1.,-1.,15.0405388283693));
#20175=CARTESIAN_POINT('Origin',(-1.,-1.,14.9063646801434));
#20176=CARTESIAN_POINT('',(-1.,-1.,14.9063646801434));
#20177=CARTESIAN_POINT('',(-1.,-1.,15.0405388283693));
#20178=CARTESIAN_POINT('',(-1.,1.,14.9063646801434));
#20179=CARTESIAN_POINT('',(-1.,1.,15.0405388283693));
#20180=CARTESIAN_POINT('',(-1.,-1.,14.9063646801434));
#20181=CARTESIAN_POINT('Origin',(-1.45,-1.,14.7425780747236));
#20182=CARTESIAN_POINT('',(-1.45,-1.,14.7425780747236));
#20183=CARTESIAN_POINT('',(-1.,-1.,14.9063646801434));
#20184=CARTESIAN_POINT('',(-1.45,1.,14.7425780747236));
#20185=CARTESIAN_POINT('',(-1.,1.,14.9063646801434));
#20186=CARTESIAN_POINT('',(-1.45,-1.,14.7425780747236));
#20187=CARTESIAN_POINT('Origin',(-1.45,-1.,14.5760069030711));
#20188=CARTESIAN_POINT('',(-1.45,-1.,14.5760069030711));
#20189=CARTESIAN_POINT('',(-1.45,-1.,14.7425780747236));
#20190=CARTESIAN_POINT('',(-1.45,1.,14.5760069030711));
#20191=CARTESIAN_POINT('',(-1.45,1.,14.7425780747236));
#20192=CARTESIAN_POINT('',(-1.45,-1.,14.5760069030711));
#20193=CARTESIAN_POINT('Origin',(-1.,-1.,14.4122202976513));
#20194=CARTESIAN_POINT('',(-1.,-1.,14.4122202976513));
#20195=CARTESIAN_POINT('',(-1.45,-1.,14.5760069030711));
#20196=CARTESIAN_POINT('',(-1.,1.,14.4122202976513));
#20197=CARTESIAN_POINT('',(-1.45,1.,14.5760069030711));
#20198=CARTESIAN_POINT('',(-1.,-1.,14.4122202976513));
#20199=CARTESIAN_POINT('Origin',(-1.,-1.,14.2780461494254));
#20200=CARTESIAN_POINT('',(-1.,-1.,14.2780461494254));
#20201=CARTESIAN_POINT('',(-1.,-1.,14.4122202976513));
#20202=CARTESIAN_POINT('',(-1.,1.,14.2780461494254));
#20203=CARTESIAN_POINT('',(-1.,1.,14.4122202976513));
#20204=CARTESIAN_POINT('',(-1.,-1.,14.2780461494254));
#20205=CARTESIAN_POINT('Origin',(-1.45,-1.,14.1142595440056));
#20206=CARTESIAN_POINT('',(-1.45,-1.,14.1142595440056));
#20207=CARTESIAN_POINT('',(-1.,-1.,14.2780461494254));
#20208=CARTESIAN_POINT('',(-1.45,1.,14.1142595440056));
#20209=CARTESIAN_POINT('',(-1.,1.,14.2780461494254));
#20210=CARTESIAN_POINT('',(-1.45,-1.,14.1142595440056));
#20211=CARTESIAN_POINT('Origin',(-1.45,-1.,13.9476883723531));
#20212=CARTESIAN_POINT('',(-1.45,-1.,13.9476883723531));
#20213=CARTESIAN_POINT('',(-1.45,-1.,14.1142595440056));
#20214=CARTESIAN_POINT('',(-1.45,1.,13.9476883723531));
#20215=CARTESIAN_POINT('',(-1.45,1.,14.1142595440056));
#20216=CARTESIAN_POINT('',(-1.45,-1.,13.9476883723531));
#20217=CARTESIAN_POINT('Origin',(-1.,-1.,13.7839017669334));
#20218=CARTESIAN_POINT('',(-1.,-1.,13.7839017669334));
#20219=CARTESIAN_POINT('',(-1.45,-1.,13.9476883723531));
#20220=CARTESIAN_POINT('',(-1.,1.,13.7839017669334));
#20221=CARTESIAN_POINT('',(-1.45,1.,13.9476883723531));
#20222=CARTESIAN_POINT('',(-1.,-1.,13.7839017669334));
#20223=CARTESIAN_POINT('Origin',(-1.,-1.,13.6497276187075));
#20224=CARTESIAN_POINT('',(-1.,-1.,13.6497276187075));
#20225=CARTESIAN_POINT('',(-1.,-1.,13.7839017669334));
#20226=CARTESIAN_POINT('',(-1.,1.,13.6497276187075));
#20227=CARTESIAN_POINT('',(-1.,1.,13.7839017669334));
#20228=CARTESIAN_POINT('',(-1.,-1.,13.6497276187075));
#20229=CARTESIAN_POINT('Origin',(-1.45,-1.,13.4859410132877));
#20230=CARTESIAN_POINT('',(-1.45,-1.,13.4859410132877));
#20231=CARTESIAN_POINT('',(-1.,-1.,13.6497276187075));
#20232=CARTESIAN_POINT('',(-1.45,1.,13.4859410132877));
#20233=CARTESIAN_POINT('',(-1.,1.,13.6497276187075));
#20234=CARTESIAN_POINT('',(-1.45,-1.,13.4859410132877));
#20235=CARTESIAN_POINT('Origin',(-1.45,-1.,13.3193698416352));
#20236=CARTESIAN_POINT('',(-1.45,-1.,13.3193698416352));
#20237=CARTESIAN_POINT('',(-1.45,-1.,13.4859410132877));
#20238=CARTESIAN_POINT('',(-1.45,1.,13.3193698416352));
#20239=CARTESIAN_POINT('',(-1.45,1.,13.4859410132877));
#20240=CARTESIAN_POINT('',(-1.45,-1.,13.3193698416352));
#20241=CARTESIAN_POINT('Origin',(-1.,-1.,13.1555832362154));
#20242=CARTESIAN_POINT('',(-1.,-1.,13.1555832362154));
#20243=CARTESIAN_POINT('',(-1.45,-1.,13.3193698416352));
#20244=CARTESIAN_POINT('',(-1.,1.,13.1555832362154));
#20245=CARTESIAN_POINT('',(-1.45,1.,13.3193698416352));
#20246=CARTESIAN_POINT('',(-1.,-1.,13.1555832362154));
#20247=CARTESIAN_POINT('Origin',(-1.,-1.,13.0214090879895));
#20248=CARTESIAN_POINT('',(-1.,-1.,13.0214090879895));
#20249=CARTESIAN_POINT('',(-1.,-1.,13.1555832362154));
#20250=CARTESIAN_POINT('',(-1.,1.,13.0214090879895));
#20251=CARTESIAN_POINT('',(-1.,1.,13.1555832362154));
#20252=CARTESIAN_POINT('',(-1.,-1.,13.0214090879895));
#20253=CARTESIAN_POINT('Origin',(-1.45,-1.,12.8576224825697));
#20254=CARTESIAN_POINT('',(-1.45,-1.,12.8576224825697));
#20255=CARTESIAN_POINT('',(-1.,-1.,13.0214090879895));
#20256=CARTESIAN_POINT('',(-1.45,1.,12.8576224825697));
#20257=CARTESIAN_POINT('',(-1.,1.,13.0214090879895));
#20258=CARTESIAN_POINT('',(-1.45,-1.,12.8576224825697));
#20259=CARTESIAN_POINT('Origin',(-1.45,-1.,12.6910513109172));
#20260=CARTESIAN_POINT('',(-1.45,-1.,12.6910513109172));
#20261=CARTESIAN_POINT('',(-1.45,-1.,12.8576224825697));
#20262=CARTESIAN_POINT('',(-1.45,1.,12.6910513109172));
#20263=CARTESIAN_POINT('',(-1.45,1.,12.8576224825697));
#20264=CARTESIAN_POINT('',(-1.45,-1.,12.6910513109172));
#20265=CARTESIAN_POINT('Origin',(-1.,-1.,12.5272647054974));
#20266=CARTESIAN_POINT('',(-1.,-1.,12.5272647054974));
#20267=CARTESIAN_POINT('',(-1.45,-1.,12.6910513109172));
#20268=CARTESIAN_POINT('',(-1.,1.,12.5272647054974));
#20269=CARTESIAN_POINT('',(-1.45,1.,12.6910513109172));
#20270=CARTESIAN_POINT('',(-1.,-1.,12.5272647054974));
#20271=CARTESIAN_POINT('Origin',(-1.,-1.,12.3930905572716));
#20272=CARTESIAN_POINT('',(-1.,-1.,12.3930905572716));
#20273=CARTESIAN_POINT('',(-1.,-1.,12.5272647054974));
#20274=CARTESIAN_POINT('',(-1.,1.,12.3930905572716));
#20275=CARTESIAN_POINT('',(-1.,1.,12.5272647054974));
#20276=CARTESIAN_POINT('',(-1.,-1.,12.3930905572716));
#20277=CARTESIAN_POINT('Origin',(-1.45,-1.,12.2293039518518));
#20278=CARTESIAN_POINT('',(-1.45,-1.,12.2293039518518));
#20279=CARTESIAN_POINT('',(-1.,-1.,12.3930905572716));
#20280=CARTESIAN_POINT('',(-1.45,1.,12.2293039518518));
#20281=CARTESIAN_POINT('',(-1.,1.,12.3930905572716));
#20282=CARTESIAN_POINT('',(-1.45,-1.,12.2293039518518));
#20283=CARTESIAN_POINT('Origin',(-1.45,-1.,12.0627327801993));
#20284=CARTESIAN_POINT('',(-1.45,-1.,12.0627327801993));
#20285=CARTESIAN_POINT('',(-1.45,-1.,12.2293039518518));
#20286=CARTESIAN_POINT('',(-1.45,1.,12.0627327801993));
#20287=CARTESIAN_POINT('',(-1.45,1.,12.2293039518518));
#20288=CARTESIAN_POINT('',(-1.45,-1.,12.0627327801993));
#20289=CARTESIAN_POINT('Origin',(-1.,-1.,11.8989461747795));
#20290=CARTESIAN_POINT('',(-1.,-1.,11.8989461747795));
#20291=CARTESIAN_POINT('',(-1.45,-1.,12.0627327801993));
#20292=CARTESIAN_POINT('',(-1.,1.,11.8989461747795));
#20293=CARTESIAN_POINT('',(-1.45,1.,12.0627327801993));
#20294=CARTESIAN_POINT('',(-1.,-1.,11.8989461747795));
#20295=CARTESIAN_POINT('Origin',(-1.,-1.,11.7647720265536));
#20296=CARTESIAN_POINT('',(-1.,-1.,11.7647720265536));
#20297=CARTESIAN_POINT('',(-1.,-1.,11.8989461747795));
#20298=CARTESIAN_POINT('',(-1.,1.,11.7647720265536));
#20299=CARTESIAN_POINT('',(-1.,1.,11.8989461747795));
#20300=CARTESIAN_POINT('',(-1.,-1.,11.7647720265536));
#20301=CARTESIAN_POINT('Origin',(-1.45,-1.,11.6009854211338));
#20302=CARTESIAN_POINT('',(-1.45,-1.,11.6009854211338));
#20303=CARTESIAN_POINT('',(-1.,-1.,11.7647720265536));
#20304=CARTESIAN_POINT('',(-1.45,1.,11.6009854211338));
#20305=CARTESIAN_POINT('',(-1.,1.,11.7647720265536));
#20306=CARTESIAN_POINT('',(-1.45,-1.,11.6009854211338));
#20307=CARTESIAN_POINT('Origin',(-1.45,-1.,11.4344142494813));
#20308=CARTESIAN_POINT('',(-1.45,-1.,11.4344142494813));
#20309=CARTESIAN_POINT('',(-1.45,-1.,11.6009854211338));
#20310=CARTESIAN_POINT('',(-1.45,1.,11.4344142494813));
#20311=CARTESIAN_POINT('',(-1.45,1.,11.6009854211338));
#20312=CARTESIAN_POINT('',(-1.45,-1.,11.4344142494813));
#20313=CARTESIAN_POINT('Origin',(-1.,-1.,11.2706276440615));
#20314=CARTESIAN_POINT('',(-1.,-1.,11.2706276440615));
#20315=CARTESIAN_POINT('',(-1.45,-1.,11.4344142494813));
#20316=CARTESIAN_POINT('',(-1.,1.,11.2706276440615));
#20317=CARTESIAN_POINT('',(-1.45,1.,11.4344142494813));
#20318=CARTESIAN_POINT('',(-1.,-1.,11.2706276440615));
#20319=CARTESIAN_POINT('Origin',(-1.,-1.,11.));
#20320=CARTESIAN_POINT('',(-1.,-1.,11.2706276440615));
#20321=CARTESIAN_POINT('',(-1.,1.,11.2706276440615));
#20322=CARTESIAN_POINT('Origin',(-0.625,1.,24.));
#20323=CARTESIAN_POINT('Origin',(-0.625,-1.,24.));
#20324=CARTESIAN_POINT('Origin',(1.,0.,10.8));
#20325=CARTESIAN_POINT('',(0.,-1.22464679914735E-16,40.));
#20326=CARTESIAN_POINT('Origin',(1.,0.,40.));
#20327=CARTESIAN_POINT('',(0.,-1.22464679914735E-16,10.8));
#20328=CARTESIAN_POINT('',(0.,-1.22464679914735E-16,10.8));
#20329=CARTESIAN_POINT('',(0.,-1.22464679914735E-16,10.8));
#20330=CARTESIAN_POINT('Origin',(1.,0.,10.8));
#20331=CARTESIAN_POINT('Origin',(1.,0.,40.));
#20332=CARTESIAN_POINT('Origin',(1.,0.,10.8));
#20333=CARTESIAN_POINT('',(0.,0.,0.));
#20334=CARTESIAN_POINT('Origin',(1.,0.,10.8));
#20335=CARTESIAN_POINT('',(0.5,-6.12323399573677E-17,11.8));
#20336=CARTESIAN_POINT('Origin',(1.,0.,11.8));
#20337=CARTESIAN_POINT('',(0.5,-6.12323399573677E-17,10.8));
#20338=CARTESIAN_POINT('',(0.5,-6.12323399573677E-17,10.8));
#20339=CARTESIAN_POINT('Origin',(1.,0.,10.8));
#20340=CARTESIAN_POINT('Origin',(1.,0.,11.8));
#20341=CARTESIAN_POINT('Origin',(1.,0.,10.));
#20342=CARTESIAN_POINT('',(-0.2,-1.46957615897682E-16,10.8));
#20343=CARTESIAN_POINT('Origin',(1.,0.,10.8));
#20344=CARTESIAN_POINT('',(-0.2,-1.46957615897682E-16,10.));
#20345=CARTESIAN_POINT('',(-0.2,-1.46957615897682E-16,10.));
#20346=CARTESIAN_POINT('Origin',(1.,0.,10.));
#20347=CARTESIAN_POINT('Origin',(1.,0.,10.8));
#20348=CARTESIAN_POINT('Origin',(1.,0.,10.));
#20349=CARTESIAN_POINT('',(0.,0.,0.));
#20350=CARTESIAN_POINT('Origin',(1.99,0.,34.));
#20351=CARTESIAN_POINT('',(1.9913626985115,0.164999999999999,34.));
#20352=CARTESIAN_POINT('',(2.005,3.8468921234385E-17,34.165));
#20353=CARTESIAN_POINT('Ctrl Pts',(1.9913626985115,0.164999999999999,34.));
#20354=CARTESIAN_POINT('Ctrl Pts',(1.9913626985115,0.164999999999999,34.0207584616532));
#20355=CARTESIAN_POINT('Ctrl Pts',(1.99208213234536,0.160843707720235,34.0428743626922));
#20356=CARTESIAN_POINT('Ctrl Pts',(1.99466757507705,0.143993298000807,34.0835155100945));
#20357=CARTESIAN_POINT('Ctrl Pts',(1.9964948147884,0.131301190829394,34.1020440469622));
#20358=CARTESIAN_POINT('Ctrl Pts',(1.99991441892026,0.102044414577984,34.1313008232136));
#20359=CARTESIAN_POINT('Ctrl Pts',(2.00173085232892,0.0835157197655827,
34.1439932187437));
#20360=CARTESIAN_POINT('Ctrl Pts',(2.00429148829838,0.0428740302308147,
34.1608438378879));
#20361=CARTESIAN_POINT('Ctrl Pts',(2.005,0.0207579399932883,34.165));
#20362=CARTESIAN_POINT('Ctrl Pts',(2.005,-4.78783679369599E-16,34.165));
#20363=CARTESIAN_POINT('Ctrl Pts',(2.005,9.0205620750794E-17,34.165));
#20364=CARTESIAN_POINT('Ctrl Pts',(2.005,-0.0207579399932887,34.165));
#20365=CARTESIAN_POINT('Ctrl Pts',(2.00429148829838,-0.0428740302308147,
34.1608438378879));
#20366=CARTESIAN_POINT('Ctrl Pts',(2.00173085232892,-0.0835157197655826,
34.1439932187437));
#20367=CARTESIAN_POINT('Ctrl Pts',(1.99991441892026,-0.102044414577984,
34.1313008232136));
#20368=CARTESIAN_POINT('Ctrl Pts',(1.9964948147884,-0.131301190829394,34.1020440469622));
#20369=CARTESIAN_POINT('Ctrl Pts',(1.99466757507705,-0.143993298000807,
34.0835155100945));
#20370=CARTESIAN_POINT('Ctrl Pts',(1.99208213234536,-0.160843707720235,
34.0428743626922));
#20371=CARTESIAN_POINT('Ctrl Pts',(1.9913626985115,-0.164999999999999,34.0207584616532));
#20372=CARTESIAN_POINT('Ctrl Pts',(1.9913626985115,-0.164999999999999,33.9792415383468));
#20373=CARTESIAN_POINT('Ctrl Pts',(1.99208213234536,-0.160843707720235,
33.9571256373078));
#20374=CARTESIAN_POINT('Ctrl Pts',(1.99466757507705,-0.143993298000807,
33.9164844899055));
#20375=CARTESIAN_POINT('Ctrl Pts',(1.9964948147884,-0.131301190829394,33.8979559530378));
#20376=CARTESIAN_POINT('Ctrl Pts',(1.99991441892026,-0.102044414577984,
33.8686991767864));
#20377=CARTESIAN_POINT('Ctrl Pts',(2.00173085232892,-0.0835157197655827,
33.8560067812563));
#20378=CARTESIAN_POINT('Ctrl Pts',(2.00429148829838,-0.0428740302308147,
33.8391561621121));
#20379=CARTESIAN_POINT('Ctrl Pts',(2.005,-0.0207579399932888,33.835));
#20380=CARTESIAN_POINT('Ctrl Pts',(2.005,0.0207579399932888,33.835));
#20381=CARTESIAN_POINT('Ctrl Pts',(2.00429148829838,0.0428740302308147,
33.8391561621121));
#20382=CARTESIAN_POINT('Ctrl Pts',(2.00173085232892,0.0835157197655826,
33.8560067812563));
#20383=CARTESIAN_POINT('Ctrl Pts',(1.99991441892026,0.102044414577984,33.8686991767864));
#20384=CARTESIAN_POINT('Ctrl Pts',(1.9964948147884,0.131301190829394,33.8979559530378));
#20385=CARTESIAN_POINT('Ctrl Pts',(1.99466757507705,0.143993298000807,33.9164844899055));
#20386=CARTESIAN_POINT('Ctrl Pts',(1.99208213234536,0.160843707720235,33.9571256373078));
#20387=CARTESIAN_POINT('Ctrl Pts',(1.9913626985115,0.164999999999999,33.9792415383468));
#20388=CARTESIAN_POINT('Ctrl Pts',(1.9913626985115,0.164999999999999,34.));
#20389=CARTESIAN_POINT('',(2.7,-2.02066721859312E-17,34.165));
#20390=CARTESIAN_POINT('',(1.99,-2.02066721859312E-17,34.165));
#20391=CARTESIAN_POINT('',(2.69197369955919,0.164999999999999,34.));
#20392=CARTESIAN_POINT('Ctrl Pts',(2.69197369955919,0.164999999999999,34.));
#20393=CARTESIAN_POINT('Ctrl Pts',(2.69197369955919,0.164999999999999,33.9792681899326));
#20394=CARTESIAN_POINT('Ctrl Pts',(2.69239400387291,0.160854068850875,33.9571634685398));
#20395=CARTESIAN_POINT('Ctrl Pts',(2.69391035162893,0.14401116680132,33.9165147673388));
#20396=CARTESIAN_POINT('Ctrl Pts',(2.69498430847444,0.131314908962089,33.8979696711705));
#20397=CARTESIAN_POINT('Ctrl Pts',(2.69699888419766,0.102030373034454,33.8686851352429));
#20398=CARTESIAN_POINT('Ctrl Pts',(2.69807062966546,0.0834852574625945,
33.8559888429375));
#20399=CARTESIAN_POINT('Ctrl Pts',(2.69958191522061,0.042836491374372,33.8391459150772));
#20400=CARTESIAN_POINT('Ctrl Pts',(2.7,0.0207317474782042,33.835));
#20401=CARTESIAN_POINT('Ctrl Pts',(2.7,-0.0207317474782042,33.835));
#20402=CARTESIAN_POINT('Ctrl Pts',(2.69958191522061,-0.042836491374372,
33.8391459150772));
#20403=CARTESIAN_POINT('Ctrl Pts',(2.69807062966546,-0.0834852574625945,
33.8559888429375));
#20404=CARTESIAN_POINT('Ctrl Pts',(2.69699888419766,-0.102030373034454,
33.8686851352429));
#20405=CARTESIAN_POINT('Ctrl Pts',(2.69498430847444,-0.131314908962089,
33.8979696711705));
#20406=CARTESIAN_POINT('Ctrl Pts',(2.69391035162893,-0.14401116680132,33.9165147673388));
#20407=CARTESIAN_POINT('Ctrl Pts',(2.69239400387291,-0.160854068850875,
33.9571634685398));
#20408=CARTESIAN_POINT('Ctrl Pts',(2.69197369955919,-0.164999999999999,
33.9792681899326));
#20409=CARTESIAN_POINT('Ctrl Pts',(2.69197369955919,-0.164999999999999,
34.0207318100674));
#20410=CARTESIAN_POINT('Ctrl Pts',(2.69239400387291,-0.160854068850875,
34.0428365314602));
#20411=CARTESIAN_POINT('Ctrl Pts',(2.69391035162893,-0.14401116680132,34.0834852326612));
#20412=CARTESIAN_POINT('Ctrl Pts',(2.69498430847444,-0.131314908962089,
34.1020303288295));
#20413=CARTESIAN_POINT('Ctrl Pts',(2.69699888419766,-0.102030373034454,
34.1313148647571));
#20414=CARTESIAN_POINT('Ctrl Pts',(2.69807062966546,-0.0834852574625945,
34.1440111570625));
#20415=CARTESIAN_POINT('Ctrl Pts',(2.69958191522061,-0.042836491374372,
34.1608540849228));
#20416=CARTESIAN_POINT('Ctrl Pts',(2.7,-0.0207317474782046,34.165));
#20417=CARTESIAN_POINT('Ctrl Pts',(2.7,-3.60822483003176E-16,34.165));
#20418=CARTESIAN_POINT('Ctrl Pts',(2.7,5.06539254985228E-16,34.165));
#20419=CARTESIAN_POINT('Ctrl Pts',(2.7,0.0207317474782047,34.165));
#20420=CARTESIAN_POINT('Ctrl Pts',(2.69958191522061,0.0428364913743719,
34.1608540849228));
#20421=CARTESIAN_POINT('Ctrl Pts',(2.69807062966546,0.0834852574625944,
34.1440111570625));
#20422=CARTESIAN_POINT('Ctrl Pts',(2.69699888419766,0.102030373034454,34.1313148647571));
#20423=CARTESIAN_POINT('Ctrl Pts',(2.69498430847444,0.131314908962089,34.1020303288295));
#20424=CARTESIAN_POINT('Ctrl Pts',(2.69391035162893,0.14401116680132,34.0834852326612));
#20425=CARTESIAN_POINT('Ctrl Pts',(2.69239400387291,0.160854068850875,34.0428365314602));
#20426=CARTESIAN_POINT('Ctrl Pts',(2.69197369955919,0.165,34.0207318100674));
#20427=CARTESIAN_POINT('Ctrl Pts',(2.69197369955919,0.165,34.));
#20428=CARTESIAN_POINT('Origin',(0.21,1.01,33.5));
#20429=CARTESIAN_POINT('',(0.21,1.01,33.6));
#20430=CARTESIAN_POINT('',(-0.367442869007697,1.01,33.6));
#20431=CARTESIAN_POINT('',(0.605,1.01,33.6));
#20432=CARTESIAN_POINT('',(0.21,1.01,34.4));
#20433=CARTESIAN_POINT('',(0.21,1.01,33.5));
#20434=CARTESIAN_POINT('',(-0.367442869007697,1.01,34.4));
#20435=CARTESIAN_POINT('',(0.605,1.01,34.4));
#20436=CARTESIAN_POINT('',(-0.367442869007697,1.01,33.6));
#20437=CARTESIAN_POINT('Origin',(0.21,-1.01,33.5));
#20438=CARTESIAN_POINT('',(0.21,-1.01,33.6));
#20439=CARTESIAN_POINT('',(0.21,-0.621228621362538,33.6));
#20440=CARTESIAN_POINT('',(0.21,-0.505,33.6));
#20441=CARTESIAN_POINT('',(0.21,-1.01,34.4));
#20442=CARTESIAN_POINT('',(0.21,-1.01,33.5));
#20443=CARTESIAN_POINT('',(0.21,-0.621228621362538,34.4));
#20444=CARTESIAN_POINT('',(0.21,-0.505,34.4));
#20445=CARTESIAN_POINT('',(0.21,-0.621228621362538,33.6));
#20446=CARTESIAN_POINT('Origin',(0.21,-1.01,33.5));
#20447=CARTESIAN_POINT('',(0.21,0.621228621362538,33.6));
#20448=CARTESIAN_POINT('',(0.21,-0.505,33.6));
#20449=CARTESIAN_POINT('',(0.21,0.621228621362538,34.4));
#20450=CARTESIAN_POINT('',(0.21,0.621228621362538,33.6));
#20451=CARTESIAN_POINT('',(0.21,-0.505,34.4));
#20452=CARTESIAN_POINT('Origin',(-0.8,-1.01,33.5));
#20453=CARTESIAN_POINT('',(-0.367442869007697,-1.01,33.6));
#20454=CARTESIAN_POINT('',(0.1,-1.01,33.6));
#20455=CARTESIAN_POINT('',(-0.367442869007697,-1.01,34.4));
#20456=CARTESIAN_POINT('',(-0.367442869007697,-1.01,33.6));
#20457=CARTESIAN_POINT('',(0.1,-1.01,34.4));
#20458=CARTESIAN_POINT('Origin',(1.,0.,34.4));
#20459=CARTESIAN_POINT('Origin',(1.,0.,34.4));
#20460=CARTESIAN_POINT('Origin',(1.,0.,34.4));
#20461=CARTESIAN_POINT('Origin',(1.,0.,33.6));
#20462=CARTESIAN_POINT('Origin',(1.,0.,33.6));
#20463=CARTESIAN_POINT('Origin',(1.,0.,33.6));
#20464=CARTESIAN_POINT('Origin',(1.,0.,33.6));
#20465=CARTESIAN_POINT('Origin',(1.,0.,33.6));
#20466=CARTESIAN_POINT('',(0.,0.,0.));
#20467=CARTESIAN_POINT('Origin',(0.0577350269189626,0.,-0.1));
#20468=CARTESIAN_POINT('',(0.0577350269189626,0.,-0.1));
#20469=CARTESIAN_POINT('',(0.115470053837925,0.,0.));
#20470=CARTESIAN_POINT('',(0.0934187836487032,0.,-0.0381939203391614));
#20471=CARTESIAN_POINT('',(0.0577350269189626,-0.2,-0.1));
#20472=CARTESIAN_POINT('',(0.0577350269189626,0.,-0.1));
#20473=CARTESIAN_POINT('',(0.115470053837925,-0.2,0.));
#20474=CARTESIAN_POINT('',(0.115470053837925,-0.2,0.));
#20475=CARTESIAN_POINT('',(0.115470053837925,0.,0.));
#20476=CARTESIAN_POINT('Origin',(-0.0577350269189626,0.,-0.1));
#20477=CARTESIAN_POINT('',(-0.0577350269189626,0.,-0.1));
#20478=CARTESIAN_POINT('',(0.0561324865405187,0.,-0.1));
#20479=CARTESIAN_POINT('',(-0.0577350269189626,-0.2,-0.1));
#20480=CARTESIAN_POINT('',(-0.0577350269189626,0.,-0.1));
#20481=CARTESIAN_POINT('',(0.0577350269189626,-0.2,-0.1));
#20482=CARTESIAN_POINT('Origin',(-0.115470053837925,0.,-1.38777878078145E-17));
#20483=CARTESIAN_POINT('',(-0.115470053837925,0.,-1.41410031829988E-17));
#20484=CARTESIAN_POINT('',(-0.0797862971081845,0.,-0.0618060796608387));
#20485=CARTESIAN_POINT('',(-0.115470053837925,-0.2,-1.38777878078145E-17));
#20486=CARTESIAN_POINT('',(-0.115470053837925,0.,-1.41410031829988E-17));
#20487=CARTESIAN_POINT('',(-0.0577350269189626,-0.2,-0.1));
#20488=CARTESIAN_POINT('Origin',(-0.0577350269189626,0.,0.1));
#20489=CARTESIAN_POINT('',(-0.0577350269189626,0.,0.1));
#20490=CARTESIAN_POINT('',(-0.0509187836487033,0.,0.111806079660839));
#20491=CARTESIAN_POINT('',(-0.0577350269189626,-0.2,0.1));
#20492=CARTESIAN_POINT('',(-0.0577350269189626,0.,0.1));
#20493=CARTESIAN_POINT('',(-0.115470053837925,-0.2,-1.41410031829988E-17));
#20494=CARTESIAN_POINT('Origin',(0.0577350269189626,0.,0.1));
#20495=CARTESIAN_POINT('',(0.0577350269189626,0.,0.1));
#20496=CARTESIAN_POINT('',(0.113867513459481,0.,0.1));
#20497=CARTESIAN_POINT('',(0.0577350269189626,-0.2,0.1));
#20498=CARTESIAN_POINT('',(0.0577350269189626,0.,0.1));
#20499=CARTESIAN_POINT('',(-0.0577350269189626,-0.2,0.1));
#20500=CARTESIAN_POINT('Origin',(0.115470053837925,0.,0.));
#20501=CARTESIAN_POINT('',(0.122286297108185,0.,-0.0118060796608386));
#20502=CARTESIAN_POINT('',(0.0577350269189626,-0.2,0.1));
#20503=CARTESIAN_POINT('Origin',(0.,-0.2,0.));
#20504=CARTESIAN_POINT('Origin',(0.17,0.,0.));
#20505=CARTESIAN_POINT('',(-0.17,-8.67361737988404E-18,-2.0818995585505E-17));
#20506=CARTESIAN_POINT('Origin',(0.,0.,0.));
#20507=CARTESIAN_POINT('Origin',(0.,-0.015,0.));
#20508=CARTESIAN_POINT('',(-0.1954,-0.0254,-2.39295984553393E-17));
#20509=CARTESIAN_POINT('Origin',(0.,-0.0254,0.));
#20510=CARTESIAN_POINT('',(-0.185,-0.015,-2.2655965784226E-17));
#20511=CARTESIAN_POINT('Origin',(0.,-0.2775,0.));
#20512=CARTESIAN_POINT('',(-0.1954,-0.5296,2.39295984553393E-17));
#20513=CARTESIAN_POINT('Origin',(0.,-0.5296,0.));
#20514=CARTESIAN_POINT('',(-0.1954,-0.2775,-2.39295984553393E-17));
#20515=CARTESIAN_POINT('Origin',(0.,-0.5625,0.));
#20516=CARTESIAN_POINT('',(-0.125,-0.6,-1.53080849893419E-17));
#20517=CARTESIAN_POINT('Origin',(0.,-0.6,0.));
#20518=CARTESIAN_POINT('',(-0.1625,-0.5625,-1.99005104861445E-17));
#20519=CARTESIAN_POINT('Origin',(0.,-0.6,0.));
#20520=CARTESIAN_POINT('',(0.,0.,0.));
#20521=CARTESIAN_POINT('',(0.,0.,0.));
#20522=CARTESIAN_POINT('',(0.,0.,0.));
#20523=CARTESIAN_POINT('',(2.6,0.,34.));
#20524=CARTESIAN_POINT('',(0.,0.,0.));
#20525=CARTESIAN_POINT('',(0.,0.,0.));
#20526=CARTESIAN_POINT('Origin',(-3.25,6.,20.));
#20527=CARTESIAN_POINT('',(-3.415,6.,20.));
#20528=CARTESIAN_POINT('Origin',(-3.25,6.,20.));
#20529=CARTESIAN_POINT('',(-3.415,7.5,20.));
#20530=CARTESIAN_POINT('',(-3.415,6.,20.));
#20531=CARTESIAN_POINT('Origin',(-3.25,7.5,20.));
#20532=CARTESIAN_POINT('Origin',(-3.25,6.,20.));
#20533=CARTESIAN_POINT('Origin',(-3.25,-5.6,20.));
#20534=CARTESIAN_POINT('',(-3.415,-5.5,20.));
#20535=CARTESIAN_POINT('Origin',(-3.25,-5.5,20.));
#20536=CARTESIAN_POINT('',(-3.415,-3.9,20.));
#20537=CARTESIAN_POINT('',(-3.415,-5.6,20.));
#20538=CARTESIAN_POINT('Origin',(-3.25,-3.9,20.));
#20539=CARTESIAN_POINT('Origin',(-3.25,-3.9,20.));
#20540=CARTESIAN_POINT('Origin',(-2.55,5.5,19.8));
#20541=CARTESIAN_POINT('',(-2.68431457505076,6.9,19.8));
#20542=CARTESIAN_POINT('',(-2.68431457505076,5.5,19.8));
#20543=CARTESIAN_POINT('',(-2.68431457505076,-5.5,19.8));
#20544=CARTESIAN_POINT('',(-2.9,6.9,19.8));
#20545=CARTESIAN_POINT('',(-2.9,6.9,19.8));
#20546=CARTESIAN_POINT('',(-2.9,5.5,19.8));
#20547=CARTESIAN_POINT('',(-2.9,5.5,19.8));
#20548=CARTESIAN_POINT('',(-2.9,5.5,19.8));
#20549=CARTESIAN_POINT('Origin',(-2.725,5.5,20.));
#20550=CARTESIAN_POINT('',(-2.68431457505076,5.5,20.2));
#20551=CARTESIAN_POINT('Origin',(-3.25,5.5,20.));
#20552=CARTESIAN_POINT('',(-2.9,5.5,20.2));
#20553=CARTESIAN_POINT('',(-2.9,5.5,20.2));
#20554=CARTESIAN_POINT('',(-2.55,5.5,20.2));
#20555=CARTESIAN_POINT('Origin',(-2.9,5.5,19.8));
#20556=CARTESIAN_POINT('',(-2.9,6.9,20.2));
#20557=CARTESIAN_POINT('',(-2.9,6.9,20.2));
#20558=CARTESIAN_POINT('',(-2.9,5.5,20.2));
#20559=CARTESIAN_POINT('Origin',(-2.9,5.5,20.2));
#20560=CARTESIAN_POINT('',(-2.68431457505076,6.9,20.2));
#20561=CARTESIAN_POINT('',(-2.68431457505076,-5.5,20.2));
#20562=CARTESIAN_POINT('',(-2.55,6.9,20.2));
#20563=CARTESIAN_POINT('Origin',(-2.725,6.9,20.));
#20564=CARTESIAN_POINT('Origin',(-3.25,6.9,20.));
#20565=CARTESIAN_POINT('Origin',(-2.55,-0.2,19.8));
#20566=CARTESIAN_POINT('',(-2.68431457505076,1.2,19.8));
#20567=CARTESIAN_POINT('',(-2.68431457505076,-0.2,19.8));
#20568=CARTESIAN_POINT('',(-2.68431457505076,-5.5,19.8));
#20569=CARTESIAN_POINT('',(-2.9,1.2,19.8));
#20570=CARTESIAN_POINT('',(-2.9,1.2,19.8));
#20571=CARTESIAN_POINT('',(-2.9,-0.2,19.8));
#20572=CARTESIAN_POINT('',(-2.9,-0.2,19.8));
#20573=CARTESIAN_POINT('',(-2.9,-0.2,19.8));
#20574=CARTESIAN_POINT('Origin',(-2.725,-0.2,20.));
#20575=CARTESIAN_POINT('',(-2.68431457505076,-0.2,20.2));
#20576=CARTESIAN_POINT('Origin',(-3.25,-0.2,20.));
#20577=CARTESIAN_POINT('',(-2.9,-0.2,20.2));
#20578=CARTESIAN_POINT('',(-2.9,-0.2,20.2));
#20579=CARTESIAN_POINT('',(-2.55,-0.2,20.2));
#20580=CARTESIAN_POINT('Origin',(-2.9,-0.2,19.8));
#20581=CARTESIAN_POINT('',(-2.9,1.2,20.2));
#20582=CARTESIAN_POINT('',(-2.9,1.2,20.2));
#20583=CARTESIAN_POINT('',(-2.9,-0.2,20.2));
#20584=CARTESIAN_POINT('Origin',(-2.9,-0.2,20.2));
#20585=CARTESIAN_POINT('',(-2.68431457505076,1.2,20.2));
#20586=CARTESIAN_POINT('',(-2.68431457505076,-5.5,20.2));
#20587=CARTESIAN_POINT('',(-2.55,1.2,20.2));
#20588=CARTESIAN_POINT('Origin',(-2.725,1.2,20.));
#20589=CARTESIAN_POINT('Origin',(-3.25,1.2,20.));
#20590=CARTESIAN_POINT('Origin',(-3.25,-5.5,20.));
#20591=CARTESIAN_POINT('',(-3.85,7.5,20.));
#20592=CARTESIAN_POINT('Origin',(-3.25,7.5,20.));
#20593=CARTESIAN_POINT('',(-3.85,-5.5,20.));
#20594=CARTESIAN_POINT('',(-3.85,-5.5,20.));
#20595=CARTESIAN_POINT('Origin',(-3.25,-5.5,20.));
#20596=CARTESIAN_POINT('Origin',(-3.25,7.5,20.));
#20597=CARTESIAN_POINT('Origin',(-3.25,-5.5,20.));
#20598=CARTESIAN_POINT('',(0.,0.,0.));
#20599=CARTESIAN_POINT('Origin',(-3.25,-5.5,20.));
#20600=CARTESIAN_POINT('',(-3.855,-3.5,20.));
#20601=CARTESIAN_POINT('Origin',(-3.25,-3.5,20.));
#20602=CARTESIAN_POINT('',(-3.855,-5.5,20.));
#20603=CARTESIAN_POINT('',(-3.855,-5.5,20.));
#20604=CARTESIAN_POINT('Origin',(-3.25,-5.5,20.));
#20605=CARTESIAN_POINT('Origin',(-3.25,-5.5,20.));
#20606=CARTESIAN_POINT('',(-4.05,-3.5,20.));
#20607=CARTESIAN_POINT('Origin',(-3.25,-3.5,20.));
#20608=CARTESIAN_POINT('',(-4.05,-5.5,20.));
#20609=CARTESIAN_POINT('',(-4.05,-5.5,20.));
#20610=CARTESIAN_POINT('Origin',(-3.25,-5.5,20.));
#20611=CARTESIAN_POINT('Origin',(-3.25,-3.5,20.));
#20612=CARTESIAN_POINT('Origin',(-3.25,-5.5,20.));
#20613=CARTESIAN_POINT('',(0.,0.,0.));
#20614=CARTESIAN_POINT('Origin',(-3.25,-2.5,20.));
#20615=CARTESIAN_POINT('',(-3.855,-1.,20.));
#20616=CARTESIAN_POINT('Origin',(-3.25,-1.,20.));
#20617=CARTESIAN_POINT('',(-3.855,-2.5,20.));
#20618=CARTESIAN_POINT('',(-3.855,-2.5,20.));
#20619=CARTESIAN_POINT('Origin',(-3.25,-2.5,20.));
#20620=CARTESIAN_POINT('Origin',(-3.25,-2.5,20.));
#20621=CARTESIAN_POINT('',(-4.05,-1.,20.));
#20622=CARTESIAN_POINT('Origin',(-3.25,-1.,20.));
#20623=CARTESIAN_POINT('',(-4.05,-2.5,20.));
#20624=CARTESIAN_POINT('',(-4.05,-2.5,20.));
#20625=CARTESIAN_POINT('Origin',(-3.25,-2.5,20.));
#20626=CARTESIAN_POINT('Origin',(-3.25,-1.,20.));
#20627=CARTESIAN_POINT('Origin',(-3.25,-2.5,20.));
#20628=CARTESIAN_POINT('',(0.,0.,0.));
#20629=CARTESIAN_POINT('Origin',(-3.25,2.2,20.));
#20630=CARTESIAN_POINT('',(-3.855,2.5,20.));
#20631=CARTESIAN_POINT('Origin',(-3.25,2.5,20.));
#20632=CARTESIAN_POINT('',(-3.855,2.2,20.));
#20633=CARTESIAN_POINT('',(-3.855,2.2,20.));
#20634=CARTESIAN_POINT('Origin',(-3.25,2.2,20.));
#20635=CARTESIAN_POINT('Origin',(-3.25,2.2,20.));
#20636=CARTESIAN_POINT('',(-4.05,2.5,20.));
#20637=CARTESIAN_POINT('Origin',(-3.25,2.5,20.));
#20638=CARTESIAN_POINT('',(-4.05,2.2,20.));
#20639=CARTESIAN_POINT('',(-4.05,2.2,20.));
#20640=CARTESIAN_POINT('Origin',(-3.25,2.2,20.));
#20641=CARTESIAN_POINT('Origin',(-3.25,2.5,20.));
#20642=CARTESIAN_POINT('Origin',(-3.25,2.2,20.));
#20643=CARTESIAN_POINT('',(0.,0.,0.));
#20644=CARTESIAN_POINT('Origin',(-3.25,3.5,20.));
#20645=CARTESIAN_POINT('',(-3.855,5.,20.));
#20646=CARTESIAN_POINT('Origin',(-3.25,5.,20.));
#20647=CARTESIAN_POINT('',(-3.855,3.5,20.));
#20648=CARTESIAN_POINT('',(-3.855,3.5,20.));
#20649=CARTESIAN_POINT('Origin',(-3.25,3.5,20.));
#20650=CARTESIAN_POINT('Origin',(-3.25,3.5,20.));
#20651=CARTESIAN_POINT('',(-4.05,5.,20.));
#20652=CARTESIAN_POINT('Origin',(-3.25,5.,20.));
#20653=CARTESIAN_POINT('',(-4.05,3.5,20.));
#20654=CARTESIAN_POINT('',(-4.05,3.5,20.));
#20655=CARTESIAN_POINT('Origin',(-3.25,3.5,20.));
#20656=CARTESIAN_POINT('Origin',(-3.25,5.,20.));
#20657=CARTESIAN_POINT('Origin',(-3.25,3.5,20.));
#20658=CARTESIAN_POINT('',(0.,0.,0.));
#20659=CARTESIAN_POINT('Origin',(-2.5,1.2,19.8));
#20660=CARTESIAN_POINT('',(-2.5,1.2,19.8));
#20661=CARTESIAN_POINT('',(-2.9,1.2,19.8));
#20662=CARTESIAN_POINT('',(-2.5,1.2,19.8));
#20663=CARTESIAN_POINT('',(-2.9,1.2,20.2));
#20664=CARTESIAN_POINT('',(-2.9,1.2,19.8));
#20665=CARTESIAN_POINT('',(-2.5,1.2,20.2));
#20666=CARTESIAN_POINT('',(-2.5,1.2,20.2));
#20667=CARTESIAN_POINT('',(-2.5,1.2,19.8));
#20668=CARTESIAN_POINT('Origin',(-2.5,-0.2,19.8));
#20669=CARTESIAN_POINT('',(-2.5,-0.2,19.8));
#20670=CARTESIAN_POINT('',(-2.5,-0.2,19.8));
#20671=CARTESIAN_POINT('',(-2.5,-0.2,20.2));
#20672=CARTESIAN_POINT('',(-2.5,-0.2,20.2));
#20673=CARTESIAN_POINT('',(-2.5,-0.2,19.8));
#20674=CARTESIAN_POINT('Origin',(-2.9,-0.2,19.8));
#20675=CARTESIAN_POINT('',(-2.9,-0.2,19.8));
#20676=CARTESIAN_POINT('',(-2.9,-0.2,19.8));
#20677=CARTESIAN_POINT('',(-2.9,-0.2,20.2));
#20678=CARTESIAN_POINT('',(-2.9,-0.2,20.2));
#20679=CARTESIAN_POINT('',(-2.9,-0.2,19.8));
#20680=CARTESIAN_POINT('Origin',(-2.9,1.2,19.8));
#20681=CARTESIAN_POINT('',(-2.9,1.2,19.8));
#20682=CARTESIAN_POINT('',(-2.9,1.2,20.2));
#20683=CARTESIAN_POINT('Origin',(-2.7,0.5,20.2));
#20684=CARTESIAN_POINT('Origin',(-2.7,0.5,19.8));
#20685=CARTESIAN_POINT('',(0.,0.,0.));
#20686=CARTESIAN_POINT('Origin',(-2.5,6.9,19.8));
#20687=CARTESIAN_POINT('',(-2.5,6.9,19.8));
#20688=CARTESIAN_POINT('',(-2.9,6.9,19.8));
#20689=CARTESIAN_POINT('',(-2.5,6.9,19.8));
#20690=CARTESIAN_POINT('',(-2.9,6.9,20.2));
#20691=CARTESIAN_POINT('',(-2.9,6.9,19.8));
#20692=CARTESIAN_POINT('',(-2.5,6.9,20.2));
#20693=CARTESIAN_POINT('',(-2.5,6.9,20.2));
#20694=CARTESIAN_POINT('',(-2.5,6.9,19.8));
#20695=CARTESIAN_POINT('Origin',(-2.5,5.5,19.8));
#20696=CARTESIAN_POINT('',(-2.5,5.5,19.8));
#20697=CARTESIAN_POINT('',(-2.5,5.5,19.8));
#20698=CARTESIAN_POINT('',(-2.5,5.5,20.2));
#20699=CARTESIAN_POINT('',(-2.5,5.5,20.2));
#20700=CARTESIAN_POINT('',(-2.5,5.5,19.8));
#20701=CARTESIAN_POINT('Origin',(-2.9,5.5,19.8));
#20702=CARTESIAN_POINT('',(-2.9,5.5,19.8));
#20703=CARTESIAN_POINT('',(-2.9,5.5,19.8));
#20704=CARTESIAN_POINT('',(-2.9,5.5,20.2));
#20705=CARTESIAN_POINT('',(-2.9,5.5,20.2));
#20706=CARTESIAN_POINT('',(-2.9,5.5,19.8));
#20707=CARTESIAN_POINT('Origin',(-2.9,6.9,19.8));
#20708=CARTESIAN_POINT('',(-2.9,6.9,19.8));
#20709=CARTESIAN_POINT('',(-2.9,6.9,20.2));
#20710=CARTESIAN_POINT('Origin',(-2.7,6.2,20.2));
#20711=CARTESIAN_POINT('Origin',(-2.7,6.2,19.8));
#20712=CARTESIAN_POINT('',(0.,0.,0.));
#20713=CARTESIAN_POINT('Origin',(-3.25,5.9,29.));
#20714=CARTESIAN_POINT('',(-3.5,6.,29.));
#20715=CARTESIAN_POINT('Origin',(-3.25,6.,29.));
#20716=CARTESIAN_POINT('',(-3.5,6.8,29.));
#20717=CARTESIAN_POINT('',(-3.5,5.9,29.));
#20718=CARTESIAN_POINT('Origin',(-3.25,6.8,29.));
#20719=CARTESIAN_POINT('Origin',(-2.47,4.9,19.8));
#20720=CARTESIAN_POINT('',(-2.47,5.,19.8));
#20721=CARTESIAN_POINT('',(-2.68431457505076,5.,19.8));
#20722=CARTESIAN_POINT('',(-2.86,5.,19.8));
#20723=CARTESIAN_POINT('',(-2.47,7.5,19.8));
#20724=CARTESIAN_POINT('',(-2.47,4.9,19.8));
#20725=CARTESIAN_POINT('',(-2.68431457505076,7.5,19.8));
#20726=CARTESIAN_POINT('',(-2.86,7.5,19.8));
#20727=CARTESIAN_POINT('',(-2.68431457505076,5.,19.8));
#20728=CARTESIAN_POINT('Origin',(-2.47,4.9,20.2));
#20729=CARTESIAN_POINT('',(-2.47,5.,20.2));
#20730=CARTESIAN_POINT('',(-2.47,5.,20.1));
#20731=CARTESIAN_POINT('',(-2.47,7.5,20.2));
#20732=CARTESIAN_POINT('',(-2.47,4.9,20.2));
#20733=CARTESIAN_POINT('',(-2.47,7.5,20.1));
#20734=CARTESIAN_POINT('Origin',(-2.9,4.9,20.2));
#20735=CARTESIAN_POINT('',(-2.68431457505076,5.,20.2));
#20736=CARTESIAN_POINT('',(-3.075,5.,20.2));
#20737=CARTESIAN_POINT('',(-2.68431457505076,7.5,20.2));
#20738=CARTESIAN_POINT('',(-2.68431457505076,5.,20.2));
#20739=CARTESIAN_POINT('',(-3.075,7.5,20.2));
#20740=CARTESIAN_POINT('Origin',(-3.25,7.5,20.));
#20741=CARTESIAN_POINT('',(-4.55,7.5,20.));
#20742=CARTESIAN_POINT('Origin',(-3.25,7.5,20.));
#20743=CARTESIAN_POINT('Origin',(-3.25,7.5,20.));
#20744=CARTESIAN_POINT('Origin',(-3.25,5.,20.));
#20745=CARTESIAN_POINT('Origin',(-3.25,5.,20.));
#20746=CARTESIAN_POINT('Origin',(-3.25,6.,29.));
#20747=CARTESIAN_POINT('',(-2.75,6.8,28.2516685226452));
#20748=CARTESIAN_POINT('',(-2.75,6.,28.2516685226452));
#20749=CARTESIAN_POINT('',(-2.75,6.,28.2516685226452));
#20750=CARTESIAN_POINT('',(-3.75,6.8,28.2516685226452));
#20751=CARTESIAN_POINT('Origin',(-3.25,6.8,29.));
#20752=CARTESIAN_POINT('',(-3.75,6.,28.2516685226452));
#20753=CARTESIAN_POINT('',(-3.75,6.,28.2516685226452));
#20754=CARTESIAN_POINT('Origin',(-3.25,6.,29.));
#20755=CARTESIAN_POINT('Origin',(-2.75,6.,29.));
#20756=CARTESIAN_POINT('',(-2.75,6.,21.2));
#20757=CARTESIAN_POINT('',(-2.75,6.,20.));
#20758=CARTESIAN_POINT('',(-2.75,6.8,21.2));
#20759=CARTESIAN_POINT('',(-2.75,5.,21.2));
#20760=CARTESIAN_POINT('',(-2.75,6.8,20.));
#20761=CARTESIAN_POINT('Origin',(-3.25,6.,24.5));
#20762=CARTESIAN_POINT('',(-3.75,6.,21.2));
#20763=CARTESIAN_POINT('',(-3.75,6.,29.));
#20764=CARTESIAN_POINT('Origin',(-3.25,6.,20.));
#20765=CARTESIAN_POINT('Origin',(-3.75,6.,20.));
#20766=CARTESIAN_POINT('',(-3.75,6.8,21.2));
#20767=CARTESIAN_POINT('',(-3.75,6.8,29.));
#20768=CARTESIAN_POINT('',(-3.75,5.,21.2));
#20769=CARTESIAN_POINT('Origin',(-3.25,6.8,24.5));
#20770=CARTESIAN_POINT('Origin',(-3.25,6.8,20.));
#20771=CARTESIAN_POINT('Origin',(-3.25,5.,20.));
#20772=CARTESIAN_POINT('',(-4.55,5.,20.));
#20773=CARTESIAN_POINT('',(-4.55,5.,20.));
#20774=CARTESIAN_POINT('Origin',(-3.25,5.,20.));
#20775=CARTESIAN_POINT('Origin',(-3.25,5.,20.));
#20776=CARTESIAN_POINT('',(0.,0.,0.));
#20777=CARTESIAN_POINT('Origin',(-3.25,6.8,29.));
#20778=CARTESIAN_POINT('',(-3.58,8.4,29.));
#20779=CARTESIAN_POINT('Origin',(-3.25,8.4,29.));
#20780=CARTESIAN_POINT('',(-3.58,6.8,29.));
#20781=CARTESIAN_POINT('',(-3.58,6.8,29.));
#20782=CARTESIAN_POINT('Origin',(-3.25,6.8,29.));
#20783=CARTESIAN_POINT('Origin',(-3.25,6.8,29.));
#20784=CARTESIAN_POINT('',(-3.65,8.4,29.));
#20785=CARTESIAN_POINT('Origin',(-3.25,8.4,29.));
#20786=CARTESIAN_POINT('',(-3.65,6.8,29.));
#20787=CARTESIAN_POINT('',(-3.65,6.8,29.));
#20788=CARTESIAN_POINT('Origin',(-3.25,6.8,29.));
#20789=CARTESIAN_POINT('Origin',(-3.25,8.4,29.));
#20790=CARTESIAN_POINT('Origin',(-3.25,6.8,29.));
#20791=CARTESIAN_POINT('',(0.,0.,0.));
#20792=CARTESIAN_POINT('Origin',(-3.25,-5.7,20.));
#20793=CARTESIAN_POINT('',(-3.475,-5.5,20.));
#20794=CARTESIAN_POINT('Origin',(-3.25,-5.5,20.));
#20795=CARTESIAN_POINT('',(-3.475,-5.7,20.));
#20796=CARTESIAN_POINT('',(-3.475,-5.7,20.));
#20797=CARTESIAN_POINT('Origin',(-3.25,-5.7,20.));
#20798=CARTESIAN_POINT('Origin',(-3.25,-5.7,20.));
#20799=CARTESIAN_POINT('',(-4.25,-5.5,20.));
#20800=CARTESIAN_POINT('Origin',(-3.25,-5.5,20.));
#20801=CARTESIAN_POINT('',(-4.25,-5.7,20.));
#20802=CARTESIAN_POINT('',(-4.25,-5.7,20.));
#20803=CARTESIAN_POINT('Origin',(-3.25,-5.7,20.));
#20804=CARTESIAN_POINT('Origin',(-3.25,-5.5,20.));
#20805=CARTESIAN_POINT('Origin',(-3.25,-5.7,20.));
#20806=CARTESIAN_POINT('',(0.,0.,0.));
#20807=CARTESIAN_POINT('Origin',(-3.25,7.5,20.));
#20808=CARTESIAN_POINT('',(-3.475,7.7,20.));
#20809=CARTESIAN_POINT('Origin',(-3.25,7.7,20.));
#20810=CARTESIAN_POINT('',(-3.475,7.5,20.));
#20811=CARTESIAN_POINT('',(-3.475,7.5,20.));
#20812=CARTESIAN_POINT('Origin',(-3.25,7.5,20.));
#20813=CARTESIAN_POINT('Origin',(-3.25,7.5,20.));
#20814=CARTESIAN_POINT('',(-4.25,7.7,20.));
#20815=CARTESIAN_POINT('Origin',(-3.25,7.7,20.));
#20816=CARTESIAN_POINT('',(-4.25,7.5,20.));
#20817=CARTESIAN_POINT('',(-4.25,7.5,20.));
#20818=CARTESIAN_POINT('Origin',(-3.25,7.5,20.));
#20819=CARTESIAN_POINT('Origin',(-3.25,7.7,20.));
#20820=CARTESIAN_POINT('Origin',(-3.25,7.5,20.));
#20821=CARTESIAN_POINT('',(0.,0.,0.));
#20822=CARTESIAN_POINT('Origin',(0.2,0.,0.));
#20823=CARTESIAN_POINT('',(0.2,2.2,-0.78));
#20824=CARTESIAN_POINT('',(0.2,2.2,-0.565685424949238));
#20825=CARTESIAN_POINT('',(0.2,2.2,0.));
#20826=CARTESIAN_POINT('',(0.2,-1.,-0.78));
#20827=CARTESIAN_POINT('',(0.2,0.,-0.78));
#20828=CARTESIAN_POINT('',(0.2,-1.,-0.565685424949238));
#20829=CARTESIAN_POINT('',(0.2,-1.,0.));
#20830=CARTESIAN_POINT('',(0.2,0.,-0.565685424949238));
#20831=CARTESIAN_POINT('Origin',(0.2,0.,-0.78));
#20832=CARTESIAN_POINT('',(-0.2,2.2,-0.78));
#20833=CARTESIAN_POINT('',(0.1,2.2,-0.78));
#20834=CARTESIAN_POINT('',(-0.2,-1.,-0.78));
#20835=CARTESIAN_POINT('',(-0.2,0.,-0.78));
#20836=CARTESIAN_POINT('',(0.1,-1.,-0.78));
#20837=CARTESIAN_POINT('Origin',(-0.2,0.,-0.78));
#20838=CARTESIAN_POINT('',(-0.2,2.2,-0.565685424949238));
#20839=CARTESIAN_POINT('',(-0.2,2.2,-0.39));
#20840=CARTESIAN_POINT('',(-0.2,-1.,-0.565685424949238));
#20841=CARTESIAN_POINT('',(-0.2,0.,-0.565685424949238));
#20842=CARTESIAN_POINT('',(-0.2,-1.,-0.39));
#20843=CARTESIAN_POINT('Origin',(0.,-1.,0.));
#20844=CARTESIAN_POINT('',(1.60662857109684,-1.,0.693717979106306));
#20845=CARTESIAN_POINT('',(1.5055822144029,-1.,0.892032620296856));
#20846=CARTESIAN_POINT('Origin',(0.,-1.,0.));
#20847=CARTESIAN_POINT('',(1.81978687191668,-1.,1.23627494547115));
#20848=CARTESIAN_POINT('Ctrl Pts',(1.5055822144029,-1.,0.892032620296856));
#20849=CARTESIAN_POINT('Ctrl Pts',(1.50980486806688,-1.,0.894452006964544));
#20850=CARTESIAN_POINT('Ctrl Pts',(1.51805569590094,-1.,0.899185047483511));
#20851=CARTESIAN_POINT('Ctrl Pts',(1.52984849887993,-1.,0.905967409625651));
#20852=CARTESIAN_POINT('Ctrl Pts',(1.54440491149498,-1.,0.914375919026456));
#20853=CARTESIAN_POINT('Ctrl Pts',(1.56065988578893,-1.,0.923832188944341));
#20854=CARTESIAN_POINT('Ctrl Pts',(1.57499388382243,-1.,0.932246680108685));
#20855=CARTESIAN_POINT('Ctrl Pts',(1.58744937487176,-1.,0.939646377893399));
#20856=CARTESIAN_POINT('Ctrl Pts',(1.59810042043673,-1.,0.946078063315257));
#20857=CARTESIAN_POINT('Ctrl Pts',(1.60706069896936,-1.,0.951613284356035));
#20858=CARTESIAN_POINT('Ctrl Pts',(1.61449324337085,-1.,0.956354422920671));
#20859=CARTESIAN_POINT('Ctrl Pts',(1.62061638140221,-1.,0.960438326101729));
#20860=CARTESIAN_POINT('Ctrl Pts',(1.62571930670187,-1.,0.964046107040536));
#20861=CARTESIAN_POINT('Ctrl Pts',(1.63013849959461,-1.,0.967387853230345));
#20862=CARTESIAN_POINT('Ctrl Pts',(1.63420665729798,-1.,0.970669715997509));
#20863=CARTESIAN_POINT('Ctrl Pts',(1.63820952658144,-1.,0.974066058287419));
#20864=CARTESIAN_POINT('Ctrl Pts',(1.64233990826687,-1.,0.977689794119417));
#20865=CARTESIAN_POINT('Ctrl Pts',(1.64665139190656,-1.,0.981562530939489));
#20866=CARTESIAN_POINT('Ctrl Pts',(1.65110016612638,-1.,0.985642622920821));
#20867=CARTESIAN_POINT('Ctrl Pts',(1.65559044289699,-1.,0.989855627854165));
#20868=CARTESIAN_POINT('Ctrl Pts',(1.66001553809947,-1.,0.994121836661306));
#20869=CARTESIAN_POINT('Ctrl Pts',(1.66430758030376,-1.,0.998389654952758));
#20870=CARTESIAN_POINT('Ctrl Pts',(1.66846059277303,-1.,1.00265091003727));
#20871=CARTESIAN_POINT('Ctrl Pts',(1.67250335383293,-1.,1.00692206696414));
#20872=CARTESIAN_POINT('Ctrl Pts',(1.67648246776464,-1.,1.01123236493511));
#20873=CARTESIAN_POINT('Ctrl Pts',(1.68044289894798,-1.,1.01561026162773));
#20874=CARTESIAN_POINT('Ctrl Pts',(1.68440578021706,-1.,1.02006795074201));
#20875=CARTESIAN_POINT('Ctrl Pts',(1.68836910178447,-1.,1.02460180535255));
#20876=CARTESIAN_POINT('Ctrl Pts',(1.69231840863458,-1.,1.02919977579147));
#20877=CARTESIAN_POINT('Ctrl Pts',(1.69623414782771,-1.,1.03384646003588));
#20878=CARTESIAN_POINT('Ctrl Pts',(1.70010052930962,-1.,1.03852922490789));
#20879=CARTESIAN_POINT('Ctrl Pts',(1.70391338707982,-1.,1.04324363334554));
#20880=CARTESIAN_POINT('Ctrl Pts',(1.70767646263649,-1.,1.04799085404995));
#20881=CARTESIAN_POINT('Ctrl Pts',(1.71139783543989,-1.,1.05277517202855));
#20882=CARTESIAN_POINT('Ctrl Pts',(1.7150865442702,-1.,1.05760163192479));
#20883=CARTESIAN_POINT('Ctrl Pts',(1.71874858456904,-1.,1.06247324680647));
#20884=CARTESIAN_POINT('Ctrl Pts',(1.72238500928453,-1.,1.06738966975462));
#20885=CARTESIAN_POINT('Ctrl Pts',(1.72599406198488,-1.,1.07234866990252));
#20886=CARTESIAN_POINT('Ctrl Pts',(1.72957248977424,-1.,1.0773470373727));
#20887=CARTESIAN_POINT('Ctrl Pts',(1.73311705663407,-1.,1.08238162784749));
#20888=CARTESIAN_POINT('Ctrl Pts',(1.73662628326091,-1.,1.08745056285427));
#20889=CARTESIAN_POINT('Ctrl Pts',(1.74010053962247,-1.,1.09255329056493));
#20890=CARTESIAN_POINT('Ctrl Pts',(1.74354119236208,-1.,1.09768999241226));
#20891=CARTESIAN_POINT('Ctrl Pts',(1.74695004214923,-1.,1.10286118991143));
#20892=CARTESIAN_POINT('Ctrl Pts',(1.7503286607592,-1.,1.10806728183007));
#20893=CARTESIAN_POINT('Ctrl Pts',(1.7536777209463,-1.,1.11330807582551));
#20894=CARTESIAN_POINT('Ctrl Pts',(1.75699720772105,-1.,1.11858293216763));
#20895=CARTESIAN_POINT('Ctrl Pts',(1.76028671825096,-1.,1.12389096855086));
#20896=CARTESIAN_POINT('Ctrl Pts',(1.7635457196617,-1.,1.12923123555075));
#20897=CARTESIAN_POINT('Ctrl Pts',(1.76677384551862,-1.,1.1346029180462));
#20898=CARTESIAN_POINT('Ctrl Pts',(1.76997111386769,-1.,1.14000548336975));
#20899=CARTESIAN_POINT('Ctrl Pts',(1.77313777896194,-1.,1.1454385822692));
#20900=CARTESIAN_POINT('Ctrl Pts',(1.7762742255701,-1.,1.15090197841515));
#20901=CARTESIAN_POINT('Ctrl Pts',(1.77938085564275,-1.,1.15639547194698));
#20902=CARTESIAN_POINT('Ctrl Pts',(1.78245795881009,-1.,1.16191881298499));
#20903=CARTESIAN_POINT('Ctrl Pts',(1.78550566040443,-1.,1.16747166312303));
#20904=CARTESIAN_POINT('Ctrl Pts',(1.78852398877616,-1.,1.17305363177328));
#20905=CARTESIAN_POINT('Ctrl Pts',(1.79151291552689,-1.,1.17866429440809));
#20906=CARTESIAN_POINT('Ctrl Pts',(1.79447240321515,-1.,1.18430321697432));
#20907=CARTESIAN_POINT('Ctrl Pts',(1.79740245923478,-1.,1.18996997934445));
#20908=CARTESIAN_POINT('Ctrl Pts',(1.80030314369879,-1.,1.19566418930242));
#20909=CARTESIAN_POINT('Ctrl Pts',(1.80317454838603,-1.,1.20138548938974));
#20910=CARTESIAN_POINT('Ctrl Pts',(1.80601678480707,-1.,1.20713356605475));
#20911=CARTESIAN_POINT('Ctrl Pts',(1.80882996917129,-1.,1.21290815708314));
#20912=CARTESIAN_POINT('Ctrl Pts',(1.81161420806656,-1.,1.21870906103557));
#20913=CARTESIAN_POINT('Ctrl Pts',(1.81436959210434,-1.,1.2245361330495));
#20914=CARTESIAN_POINT('Ctrl Pts',(1.8165508718364,-1.,1.2292186489137));
#20915=CARTESIAN_POINT('Ctrl Pts',(1.81817389921279,-1.,1.2327422452705));
#20916=CARTESIAN_POINT('Ctrl Pts',(1.81925017193666,-1.,1.23509651170476));
#20917=CARTESIAN_POINT('Ctrl Pts',(1.81978687191668,-1.,1.23627494547115));
#20918=CARTESIAN_POINT('',(1.73811241238545,-1.,1.34869019493419));
#20919=CARTESIAN_POINT('',(1.81978687191668,-1.,1.23627494547115));
#20920=CARTESIAN_POINT('',(1.31362392696032,-1.,1.15624053661742));
#20921=CARTESIAN_POINT('Ctrl Pts',(1.73811241238545,-1.,1.34869019493419));
#20922=CARTESIAN_POINT('Ctrl Pts',(1.73682580585691,-1.,1.34854391898045));
#20923=CARTESIAN_POINT('Ctrl Pts',(1.73425417885907,-1.,1.34824783112887));
#20924=CARTESIAN_POINT('Ctrl Pts',(1.7304014965394,-1.,1.34779309152035));
#20925=CARTESIAN_POINT('Ctrl Pts',(1.72527410680674,-1.,1.34716554819527));
#20926=CARTESIAN_POINT('Ctrl Pts',(1.7188807715049,-1.,1.34634568653227));
#20927=CARTESIAN_POINT('Ctrl Pts',(1.71250340686822,-1.,1.34549029589416));
#20928=CARTESIAN_POINT('Ctrl Pts',(1.70614212266738,-1.,1.34459924533831));
#20929=CARTESIAN_POINT('Ctrl Pts',(1.69979707754427,-1.,1.34367237124483));
#20930=CARTESIAN_POINT('Ctrl Pts',(1.6934684849687,-1.,1.34270948206319));
#20931=CARTESIAN_POINT('Ctrl Pts',(1.68715660868764,-1.,1.341710374848));
#20932=CARTESIAN_POINT('Ctrl Pts',(1.68086176030362,-1.,1.34067485185203));
#20933=CARTESIAN_POINT('Ctrl Pts',(1.67458429426086,-1.,1.3396027347034));
#20934=CARTESIAN_POINT('Ctrl Pts',(1.66832460783989,-1.,1.33849388654388));
#20935=CARTESIAN_POINT('Ctrl Pts',(1.66208312541983,-1.,1.33734820885262));
#20936=CARTESIAN_POINT('Ctrl Pts',(1.65586025952593,-1.,1.33616559745172));
#20937=CARTESIAN_POINT('Ctrl Pts',(1.6496563728683,-1.,1.33494590467993));
#20938=CARTESIAN_POINT('Ctrl Pts',(1.6434717485603,-1.,1.33368890676572));
#20939=CARTESIAN_POINT('Ctrl Pts',(1.63730653475089,-1.,1.33239425103724));
#20940=CARTESIAN_POINT('Ctrl Pts',(1.63116079730923,-1.,1.33106149345645));
#20941=CARTESIAN_POINT('Ctrl Pts',(1.62503464209797,-1.,1.3296901950568));
#20942=CARTESIAN_POINT('Ctrl Pts',(1.61892832270724,-1.,1.32828000610449));
#20943=CARTESIAN_POINT('Ctrl Pts',(1.6128423401575,-1.,1.32683074483356));
#20944=CARTESIAN_POINT('Ctrl Pts',(1.60677758290954,-1.,1.32534250785782));
#20945=CARTESIAN_POINT('Ctrl Pts',(1.60073511858687,-1.,1.32381550858256));
#20946=CARTESIAN_POINT('Ctrl Pts',(1.59471591079403,-1.,1.32224985747682));
#20947=CARTESIAN_POINT('Ctrl Pts',(1.58872057258245,-1.,1.32064537110892));
#20948=CARTESIAN_POINT('Ctrl Pts',(1.58274907898834,-1.,1.31900135021432));
#20949=CARTESIAN_POINT('Ctrl Pts',(1.5768005650559,-1.,1.31731642317187));
#20950=CARTESIAN_POINT('Ctrl Pts',(1.57087397835723,-1.,1.31558903860016));
#20951=CARTESIAN_POINT('Ctrl Pts',(1.56496872402353,-1.,1.31381795281002));
#20952=CARTESIAN_POINT('Ctrl Pts',(1.55908521254821,-1.,1.31200264341696));
#20953=CARTESIAN_POINT('Ctrl Pts',(1.55322568759481,-1.,1.31014393684222));
#20954=CARTESIAN_POINT('Ctrl Pts',(1.54739413957185,-1.,1.30824393907473));
#20955=CARTESIAN_POINT('Ctrl Pts',(1.54159462645432,-1.,1.30630475189556));
#20956=CARTESIAN_POINT('Ctrl Pts',(1.53582981268977,-1.,1.30432735639489));
#20957=CARTESIAN_POINT('Ctrl Pts',(1.53009970283891,-1.,1.30231064395568));
#20958=CARTESIAN_POINT('Ctrl Pts',(1.52439957861062,-1.,1.30024984366328));
#20959=CARTESIAN_POINT('Ctrl Pts',(1.51872184912724,-1.,1.29813791800747));
#20960=CARTESIAN_POINT('Ctrl Pts',(1.51305994241402,-1.,1.29596850710509));
#20961=CARTESIAN_POINT('Ctrl Pts',(1.50741159078365,-1.,1.29373841372842));
#20962=CARTESIAN_POINT('Ctrl Pts',(1.50178230149776,-1.,1.29145022885181));
#20963=CARTESIAN_POINT('Ctrl Pts',(1.49618896881754,-1.,1.28911506584254));
#20964=CARTESIAN_POINT('Ctrl Pts',(1.4906522831278,-1.,1.2867467611644));
#20965=CARTESIAN_POINT('Ctrl Pts',(1.4851881711891,-1.,1.28435533880201));
#20966=CARTESIAN_POINT('Ctrl Pts',(1.47980070347095,-1.,1.28194158939517));
#20967=CARTESIAN_POINT('Ctrl Pts',(1.4744717526707,-1.,1.2794891824849));
#20968=CARTESIAN_POINT('Ctrl Pts',(1.46916035917133,-1.,1.2769641483109));
#20969=CARTESIAN_POINT('Ctrl Pts',(1.46382431332476,-1.,1.27433119897822));
#20970=CARTESIAN_POINT('Ctrl Pts',(1.45843906294697,-1.,1.27156805265289));
#20971=CARTESIAN_POINT('Ctrl Pts',(1.45301422764247,-1.,1.2686778680489));
#20972=CARTESIAN_POINT('Ctrl Pts',(1.44761985001662,-1.,1.26570925118868));
#20973=CARTESIAN_POINT('Ctrl Pts',(1.44236470511303,-1.,1.26273903323859));
#20974=CARTESIAN_POINT('Ctrl Pts',(1.43734919180847,-1.,1.25983531012005));
#20975=CARTESIAN_POINT('Ctrl Pts',(1.43262645609691,-1.,1.25702687965755));
#20976=CARTESIAN_POINT('Ctrl Pts',(1.42815938799387,-1.,1.25426945222639));
#20977=CARTESIAN_POINT('Ctrl Pts',(1.42378102115575,-1.,1.2514145557001));
#20978=CARTESIAN_POINT('Ctrl Pts',(1.41923722596025,-1.,1.24824430986571));
#20979=CARTESIAN_POINT('Ctrl Pts',(1.41422913175179,-1.,1.24450600513056));
#20980=CARTESIAN_POINT('Ctrl Pts',(1.40845295531283,-1.,1.23994455029534));
#20981=CARTESIAN_POINT('Ctrl Pts',(1.40164708206106,-1.,1.23434087290423));
#20982=CARTESIAN_POINT('Ctrl Pts',(1.39361389568796,-1.,1.22752961899387));
#20983=CARTESIAN_POINT('Ctrl Pts',(1.38420564527715,-1.,1.21938737280852));
#20984=CARTESIAN_POINT('Ctrl Pts',(1.37331915607905,-1.,1.20982812925645));
#20985=CARTESIAN_POINT('Ctrl Pts',(1.36088705043885,-1.,1.1987959077932));
#20986=CARTESIAN_POINT('Ctrl Pts',(1.34687054001093,-1.,1.18625865667441));
#20987=CARTESIAN_POINT('Ctrl Pts',(1.33437539347008,-1.,1.17501305789857));
#20988=CARTESIAN_POINT('Ctrl Pts',(1.32428080721772,-1.,1.16589330093588));
#20989=CARTESIAN_POINT('Ctrl Pts',(1.31722977216397,-1.,1.15950888730809));
#20990=CARTESIAN_POINT('Ctrl Pts',(1.31362392696032,-1.,1.15624053661742));
#20991=CARTESIAN_POINT('',(1.15624053661742,-1.,1.31362392696033));
#20992=CARTESIAN_POINT('Origin',(0.,-1.,0.));
#20993=CARTESIAN_POINT('',(1.34869019493419,-1.,1.73811241238545));
#20994=CARTESIAN_POINT('Ctrl Pts',(1.15624053661742,-1.,1.31362392696033));
#20995=CARTESIAN_POINT('Ctrl Pts',(1.15950888730433,-1.,1.3172297721596));
#20996=CARTESIAN_POINT('Ctrl Pts',(1.16589330092532,-1.,1.32428080720544));
#20997=CARTESIAN_POINT('Ctrl Pts',(1.17501305787994,-1.,1.33437539344842));
#20998=CARTESIAN_POINT('Ctrl Pts',(1.18625865664915,-1.,1.34687053998157));
#20999=CARTESIAN_POINT('Ctrl Pts',(1.1987959077656,-1.,1.36088705040677));
#21000=CARTESIAN_POINT('Ctrl Pts',(1.20982812923113,-1.,1.37331915604962));
#21001=CARTESIAN_POINT('Ctrl Pts',(1.21938737278853,-1.,1.38420564525391));
#21002=CARTESIAN_POINT('Ctrl Pts',(1.22752961898063,-1.,1.39361389567257));
#21003=CARTESIAN_POINT('Ctrl Pts',(1.23434087289768,-1.,1.40164708205345));
#21004=CARTESIAN_POINT('Ctrl Pts',(1.23994455029421,-1.,1.40845295531151));
#21005=CARTESIAN_POINT('Ctrl Pts',(1.24450600513278,-1.,1.41422913175437));
#21006=CARTESIAN_POINT('Ctrl Pts',(1.24824430986911,-1.,1.41923722596421));
#21007=CARTESIAN_POINT('Ctrl Pts',(1.25141455570299,-1.,1.42378102115911));
#21008=CARTESIAN_POINT('Ctrl Pts',(1.25426945222783,-1.,1.42815938799555));
#21009=CARTESIAN_POINT('Ctrl Pts',(1.25702687965744,-1.,1.43262645609679));
#21010=CARTESIAN_POINT('Ctrl Pts',(1.25983531011894,-1.,1.43734919180719));
#21011=CARTESIAN_POINT('Ctrl Pts',(1.26273903323723,-1.,1.44236470511145));
#21012=CARTESIAN_POINT('Ctrl Pts',(1.26570925118767,-1.,1.44761985001544));
#21013=CARTESIAN_POINT('Ctrl Pts',(1.26867786804854,-1.,1.45301422764205));
#21014=CARTESIAN_POINT('Ctrl Pts',(1.27156805265312,-1.,1.45843906294725));
#21015=CARTESIAN_POINT('Ctrl Pts',(1.27433119897877,-1.,1.4638243133254));
#21016=CARTESIAN_POINT('Ctrl Pts',(1.27696414831144,-1.,1.46916035917197));
#21017=CARTESIAN_POINT('Ctrl Pts',(1.27948918248524,-1.,1.4744717526711));
#21018=CARTESIAN_POINT('Ctrl Pts',(1.28194158939522,-1.,1.47980070347102));
#21019=CARTESIAN_POINT('Ctrl Pts',(1.28435533880184,-1.,1.48518817118891));
#21020=CARTESIAN_POINT('Ctrl Pts',(1.28674676116415,-1.,1.4906522831275));
#21021=CARTESIAN_POINT('Ctrl Pts',(1.28911506584232,-1.,1.49618896881729));
#21022=CARTESIAN_POINT('Ctrl Pts',(1.29145022885171,-1.,1.50178230149764));
#21023=CARTESIAN_POINT('Ctrl Pts',(1.29373841372843,-1.,1.50741159078367));
#21024=CARTESIAN_POINT('Ctrl Pts',(1.29596850710518,-1.,1.51305994241412));
#21025=CARTESIAN_POINT('Ctrl Pts',(1.29813791800757,-1.,1.51872184912735));
#21026=CARTESIAN_POINT('Ctrl Pts',(1.30024984366334,-1.,1.5243995786107));
#21027=CARTESIAN_POINT('Ctrl Pts',(1.3023106439557,-1.,1.53009970283893));
#21028=CARTESIAN_POINT('Ctrl Pts',(1.30432735639487,-1.,1.53582981268976));
#21029=CARTESIAN_POINT('Ctrl Pts',(1.30630475189553,-1.,1.54159462645428));
#21030=CARTESIAN_POINT('Ctrl Pts',(1.30824393907471,-1.,1.54739413957183));
#21031=CARTESIAN_POINT('Ctrl Pts',(1.31014393684221,-1.,1.55322568759481));
#21032=CARTESIAN_POINT('Ctrl Pts',(1.31200264341696,-1.,1.55908521254822));
#21033=CARTESIAN_POINT('Ctrl Pts',(1.31381795281002,-1.,1.56496872402352));
#21034=CARTESIAN_POINT('Ctrl Pts',(1.31558903860015,-1.,1.57087397835721));
#21035=CARTESIAN_POINT('Ctrl Pts',(1.31731642317183,-1.,1.57680056505585));
#21036=CARTESIAN_POINT('Ctrl Pts',(1.31900135021428,-1.,1.58274907898829));
#21037=CARTESIAN_POINT('Ctrl Pts',(1.32064537110891,-1.,1.58872057258244));
#21038=CARTESIAN_POINT('Ctrl Pts',(1.32224985747686,-1.,1.59471591079408));
#21039=CARTESIAN_POINT('Ctrl Pts',(1.32381550858266,-1.,1.600735118587));
#21040=CARTESIAN_POINT('Ctrl Pts',(1.32534250785794,-1.,1.6067775829097));
#21041=CARTESIAN_POINT('Ctrl Pts',(1.32683074483365,-1.,1.61284234015762));
#21042=CARTESIAN_POINT('Ctrl Pts',(1.32828000610448,-1.,1.61892832270723));
#21043=CARTESIAN_POINT('Ctrl Pts',(1.32969019505665,-1.,1.62503464209777));
#21044=CARTESIAN_POINT('Ctrl Pts',(1.33106149345618,-1.,1.63116079730887));
#21045=CARTESIAN_POINT('Ctrl Pts',(1.33239425103694,-1.,1.6373065347505));
#21046=CARTESIAN_POINT('Ctrl Pts',(1.33368890676554,-1.,1.64347174856007));
#21047=CARTESIAN_POINT('Ctrl Pts',(1.33494590468003,-1.,1.64965637286843));
#21048=CARTESIAN_POINT('Ctrl Pts',(1.33616559745217,-1.,1.65586025952651));
#21049=CARTESIAN_POINT('Ctrl Pts',(1.33734820885331,-1.,1.66208312542073));
#21050=CARTESIAN_POINT('Ctrl Pts',(1.33849388654458,-1.,1.66832460784078));
#21051=CARTESIAN_POINT('Ctrl Pts',(1.33960273470372,-1.,1.67458429426126));
#21052=CARTESIAN_POINT('Ctrl Pts',(1.3406748518516,-1.,1.68086176030308));
#21053=CARTESIAN_POINT('Ctrl Pts',(1.34171037484673,-1.,1.68715660868602));
#21054=CARTESIAN_POINT('Ctrl Pts',(1.34270948206139,-1.,1.6934684849664));
#21055=CARTESIAN_POINT('Ctrl Pts',(1.34367237124322,-1.,1.69979707754221));
#21056=CARTESIAN_POINT('Ctrl Pts',(1.34459924533783,-1.,1.70614212266676));
#21057=CARTESIAN_POINT('Ctrl Pts',(1.34549029589563,-1.,1.71250340687011));
#21058=CARTESIAN_POINT('Ctrl Pts',(1.34634568653586,-1.,1.7188807715095));
#21059=CARTESIAN_POINT('Ctrl Pts',(1.34716554820013,-1.,1.72527410681298));
#21060=CARTESIAN_POINT('Ctrl Pts',(1.3477930915247,-1.,1.73040149654497));
#21061=CARTESIAN_POINT('Ctrl Pts',(1.34824783113158,-1.,1.73425417886255));
#21062=CARTESIAN_POINT('Ctrl Pts',(1.34854391898145,-1.,1.73682580585819));
#21063=CARTESIAN_POINT('Ctrl Pts',(1.34869019493419,-1.,1.73811241238545));
#21064=CARTESIAN_POINT('',(1.23627494547115,-1.,1.81978687191668));
#21065=CARTESIAN_POINT('',(1.34869019493419,-1.,1.73811241238545));
#21066=CARTESIAN_POINT('',(0.892032620296855,-1.,1.5055822144029));
#21067=CARTESIAN_POINT('Ctrl Pts',(1.23627494547115,-1.,1.81978687191668));
#21068=CARTESIAN_POINT('Ctrl Pts',(1.23509651170384,-1.,1.81925017193531));
#21069=CARTESIAN_POINT('Ctrl Pts',(1.23274224526804,-1.,1.81817389920914));
#21070=CARTESIAN_POINT('Ctrl Pts',(1.22921864890975,-1.,1.81655087183054));
#21071=CARTESIAN_POINT('Ctrl Pts',(1.22453613304507,-1.,1.81436959209778));
#21072=CARTESIAN_POINT('Ctrl Pts',(1.2187090610323,-1.,1.81161420806172));
#21073=CARTESIAN_POINT('Ctrl Pts',(1.2129081570818,-1.,1.80882996916931));
#21074=CARTESIAN_POINT('Ctrl Pts',(1.20713356605519,-1.,1.80601678480772));
#21075=CARTESIAN_POINT('Ctrl Pts',(1.2013854893912,-1.,1.8031745483882));
#21076=CARTESIAN_POINT('Ctrl Pts',(1.19566418930405,-1.,1.80030314370121));
#21077=CARTESIAN_POINT('Ctrl Pts',(1.1899699793456,-1.,1.79740245923649));
#21078=CARTESIAN_POINT('Ctrl Pts',(1.18430321697471,-1.,1.79447240321572));
#21079=CARTESIAN_POINT('Ctrl Pts',(1.17866429440781,-1.,1.79151291552646));
#21080=CARTESIAN_POINT('Ctrl Pts',(1.17305363177265,-1.,1.78852398877523));
#21081=CARTESIAN_POINT('Ctrl Pts',(1.16747166312239,-1.,1.78550566040349));
#21082=CARTESIAN_POINT('Ctrl Pts',(1.16191881298458,-1.,1.78245795880949));
#21083=CARTESIAN_POINT('Ctrl Pts',(1.15639547194689,-1.,1.77938085564261));
#21084=CARTESIAN_POINT('Ctrl Pts',(1.15090197841531,-1.,1.77627422557034));
#21085=CARTESIAN_POINT('Ctrl Pts',(1.14543858226948,-1.,1.77313777896234));
#21086=CARTESIAN_POINT('Ctrl Pts',(1.14000548337,-1.,1.76997111386806));
#21087=CARTESIAN_POINT('Ctrl Pts',(1.13460291804634,-1.,1.76677384551883));
#21088=CARTESIAN_POINT('Ctrl Pts',(1.12923123555076,-1.,1.76354571966171));
#21089=CARTESIAN_POINT('Ctrl Pts',(1.12389096855078,-1.,1.76028671825084));
#21090=CARTESIAN_POINT('Ctrl Pts',(1.11858293216752,-1.,1.75699720772089));
#21091=CARTESIAN_POINT('Ctrl Pts',(1.11330807582542,-1.,1.75367772094617));
#21092=CARTESIAN_POINT('Ctrl Pts',(1.10806728183003,-1.,1.75032866075914));
#21093=CARTESIAN_POINT('Ctrl Pts',(1.10286118991144,-1.,1.74695004214924));
#21094=CARTESIAN_POINT('Ctrl Pts',(1.09768999241229,-1.,1.74354119236212));
#21095=CARTESIAN_POINT('Ctrl Pts',(1.09255329056496,-1.,1.74010053962252));
#21096=CARTESIAN_POINT('Ctrl Pts',(1.08745056285429,-1.,1.73662628326093));
#21097=CARTESIAN_POINT('Ctrl Pts',(1.08238162784749,-1.,1.73311705663407));
#21098=CARTESIAN_POINT('Ctrl Pts',(1.0773470373727,-1.,1.72957248977424));
#21099=CARTESIAN_POINT('Ctrl Pts',(1.07234866990252,-1.,1.72599406198489));
#21100=CARTESIAN_POINT('Ctrl Pts',(1.06738966975463,-1.,1.72238500928456));
#21101=CARTESIAN_POINT('Ctrl Pts',(1.06247324680649,-1.,1.71874858456908));
#21102=CARTESIAN_POINT('Ctrl Pts',(1.05760163192481,-1.,1.71508654427022));
#21103=CARTESIAN_POINT('Ctrl Pts',(1.05277517202853,-1.,1.71139783543986));
#21104=CARTESIAN_POINT('Ctrl Pts',(1.0479908540499,-1.,1.70767646263641));
#21105=CARTESIAN_POINT('Ctrl Pts',(1.04324363334546,-1.,1.70391338707969));
#21106=CARTESIAN_POINT('Ctrl Pts',(1.03852922490782,-1.,1.70010052930951));
#21107=CARTESIAN_POINT('Ctrl Pts',(1.03384646003587,-1.,1.69623414782769));
#21108=CARTESIAN_POINT('Ctrl Pts',(1.02919977579155,-1.,1.69231840863471));
#21109=CARTESIAN_POINT('Ctrl Pts',(1.02460180535272,-1.,1.68836910178475));
#21110=CARTESIAN_POINT('Ctrl Pts',(1.02006795074222,-1.,1.68440578021739));
#21111=CARTESIAN_POINT('Ctrl Pts',(1.01561026162786,-1.,1.6804428989482));
#21112=CARTESIAN_POINT('Ctrl Pts',(1.01123236493507,-1.,1.67648246776457));
#21113=CARTESIAN_POINT('Ctrl Pts',(1.00692206696387,-1.,1.67250335383248));
#21114=CARTESIAN_POINT('Ctrl Pts',(1.00265091003682,-1.,1.66846059277231));
#21115=CARTESIAN_POINT('Ctrl Pts',(0.998389654952317,-1.,1.66430758030304));
#21116=CARTESIAN_POINT('Ctrl Pts',(0.994121836661115,-1.,1.66001553809916));
#21117=CARTESIAN_POINT('Ctrl Pts',(0.98985562785445,-1.,1.65559044289746));
#21118=CARTESIAN_POINT('Ctrl Pts',(0.985642622921626,-1.,1.6511001661277));
#21119=CARTESIAN_POINT('Ctrl Pts',(0.981562530940574,-1.,1.64665139190834));
#21120=CARTESIAN_POINT('Ctrl Pts',(0.977689794120296,-1.,1.64233990826831));
#21121=CARTESIAN_POINT('Ctrl Pts',(0.974066058287501,-1.,1.63820952658157));
#21122=CARTESIAN_POINT('Ctrl Pts',(0.970669715996356,-1.,1.63420665729609));
#21123=CARTESIAN_POINT('Ctrl Pts',(0.967387853228041,-1.,1.63013849959083));
#21124=CARTESIAN_POINT('Ctrl Pts',(0.964046107037821,-1.,1.6257193066974));
#21125=CARTESIAN_POINT('Ctrl Pts',(0.960438326099958,-1.,1.62061638139929));
#21126=CARTESIAN_POINT('Ctrl Pts',(0.956354422921572,-1.,1.61449324337233));
#21127=CARTESIAN_POINT('Ctrl Pts',(0.951613284361247,-1.,1.60706069897794));
#21128=CARTESIAN_POINT('Ctrl Pts',(0.946078063325795,-1.,1.59810042045408));
#21129=CARTESIAN_POINT('Ctrl Pts',(0.939646377909319,-1.,1.58744937489796));
#21130=CARTESIAN_POINT('Ctrl Pts',(0.932246680128848,-1.,1.57499388385561));
#21131=CARTESIAN_POINT('Ctrl Pts',(0.923832188966322,-1.,1.56065988582509));
#21132=CARTESIAN_POINT('Ctrl Pts',(0.914375919046579,-1.,1.54440491152808));
#21133=CARTESIAN_POINT('Ctrl Pts',(0.905967409640498,-1.,1.52984849890434));
#21134=CARTESIAN_POINT('Ctrl Pts',(0.89918504749193,-1.,1.51805569591479));
#21135=CARTESIAN_POINT('Ctrl Pts',(0.894452006967538,-1.,1.50980486807181));
#21136=CARTESIAN_POINT('Ctrl Pts',(0.892032620296855,-1.,1.5055822144029));
#21137=CARTESIAN_POINT('',(0.693717979106305,-1.,1.60662857109684));
#21138=CARTESIAN_POINT('Origin',(0.,-1.,0.));
#21139=CARTESIAN_POINT('',(0.7455743247944,-1.,2.0698113262342));
#21140=CARTESIAN_POINT('Ctrl Pts',(0.693717979106305,-1.,1.60662857109684));
#21141=CARTESIAN_POINT('Ctrl Pts',(0.69571209787897,-1.,1.61106790957619));
#21142=CARTESIAN_POINT('Ctrl Pts',(0.699605146398836,-1.,1.61974673471117));
#21143=CARTESIAN_POINT('Ctrl Pts',(0.705159151977294,-1.,1.6321654166204));
#21144=CARTESIAN_POINT('Ctrl Pts',(0.711993139340447,-1.,1.64752408828442));
#21145=CARTESIAN_POINT('Ctrl Pts',(0.719585433787949,-1.,1.66472880551777));
#21146=CARTESIAN_POINT('Ctrl Pts',(0.726235967982445,-1.,1.67996158451922));
#21147=CARTESIAN_POINT('Ctrl Pts',(0.731963238685357,-1.,1.69326921972915));
#21148=CARTESIAN_POINT('Ctrl Pts',(0.736799665716932,-1.,1.70473309004249));
#21149=CARTESIAN_POINT('Ctrl Pts',(0.74079516202821,-1.,1.71447789751001));
#21150=CARTESIAN_POINT('Ctrl Pts',(0.744021445433093,-1.,1.72268229916769));
#21151=CARTESIAN_POINT('Ctrl Pts',(0.746574710097752,-1.,1.72958533647714));
#21152=CARTESIAN_POINT('Ctrl Pts',(0.74858246295687,-1.,1.7355035168033));
#21153=CARTESIAN_POINT('Ctrl Pts',(0.750193435981249,-1.,1.74080458267114));
#21154=CARTESIAN_POINT('Ctrl Pts',(0.751555614164482,-1.,1.74585086852502));
#21155=CARTESIAN_POINT('Ctrl Pts',(0.752797683531314,-1.,1.75095139468794));
#21156=CARTESIAN_POINT('Ctrl Pts',(0.754009254027828,-1.,1.75631083600019));
#21157=CARTESIAN_POINT('Ctrl Pts',(0.755220979974461,-1.,1.76197817240128));
#21158=CARTESIAN_POINT('Ctrl Pts',(0.75642189602781,-1.,1.76789396002998));
#21159=CARTESIAN_POINT('Ctrl Pts',(0.757578264077028,-1.,1.77394167108292));
#21160=CARTESIAN_POINT('Ctrl Pts',(0.758650626677518,-1.,1.77999411220945));
#21161=CARTESIAN_POINT('Ctrl Pts',(0.759614401110189,-1.,1.78596964884604));
#21162=CARTESIAN_POINT('Ctrl Pts',(0.760469555880749,-1.,1.7918581561088));
#21163=CARTESIAN_POINT('Ctrl Pts',(0.761229695230558,-1.,1.79768986997783));
#21164=CARTESIAN_POINT('Ctrl Pts',(0.761915336443547,-1.,1.80351583877342));
#21165=CARTESIAN_POINT('Ctrl Pts',(0.762546129463938,-1.,1.80938551463965));
#21166=CARTESIAN_POINT('Ctrl Pts',(0.763132003836634,-1.,1.8153211840553));
#21167=CARTESIAN_POINT('Ctrl Pts',(0.763673465462726,-1.,1.82131873145266));
#21168=CARTESIAN_POINT('Ctrl Pts',(0.764165902605995,-1.,1.82735991200065));
#21169=CARTESIAN_POINT('Ctrl Pts',(0.764602549687853,-1.,1.83342077227142));
#21170=CARTESIAN_POINT('Ctrl Pts',(0.764978057881737,-1.,1.83948181064835));
#21171=CARTESIAN_POINT('Ctrl Pts',(0.765291664862029,-1.,1.84553698875924));
#21172=CARTESIAN_POINT('Ctrl Pts',(0.765545710619062,-1.,1.85158945130063));
#21173=CARTESIAN_POINT('Ctrl Pts',(0.765744212909318,-1.,1.85764741390394));
#21174=CARTESIAN_POINT('Ctrl Pts',(0.765891519092547,-1.,1.86372027063312));
#21175=CARTESIAN_POINT('Ctrl Pts',(0.765990708546091,-1.,1.86981398314341));
#21176=CARTESIAN_POINT('Ctrl Pts',(0.766042837036744,-1.,1.87592888967883));
#21177=CARTESIAN_POINT('Ctrl Pts',(0.766047794851864,-1.,1.88206215302561));
#21178=CARTESIAN_POINT('Ctrl Pts',(0.766004837062091,-1.,1.88820926433409));
#21179=CARTESIAN_POINT('Ctrl Pts',(0.765913193856978,-1.,1.89436577771388));
#21180=CARTESIAN_POINT('Ctrl Pts',(0.765772772593386,-1.,1.90052930393596));
#21181=CARTESIAN_POINT('Ctrl Pts',(0.765584196937919,-1.,1.90669961402356));
#21182=CARTESIAN_POINT('Ctrl Pts',(0.765348465884722,-1.,1.91287765805169));
#21183=CARTESIAN_POINT('Ctrl Pts',(0.765066729667088,-1.,1.91906491634196));
#21184=CARTESIAN_POINT('Ctrl Pts',(0.764740025488211,-1.,1.92526263537048));
#21185=CARTESIAN_POINT('Ctrl Pts',(0.76436901067394,-1.,1.93147105496382));
#21186=CARTESIAN_POINT('Ctrl Pts',(0.763954049121458,-1.,1.93768964875886));
#21187=CARTESIAN_POINT('Ctrl Pts',(0.763495333538629,-1.,1.9439174661764));
#21188=CARTESIAN_POINT('Ctrl Pts',(0.762992990878769,-1.,1.95015342590024));
#21189=CARTESIAN_POINT('Ctrl Pts',(0.762447203806178,-1.,1.95639665309869));
#21190=CARTESIAN_POINT('Ctrl Pts',(0.761858300014423,-1.,1.96264672744186));
#21191=CARTESIAN_POINT('Ctrl Pts',(0.76122669048382,-1.,1.96890351582499));
#21192=CARTESIAN_POINT('Ctrl Pts',(0.760552825409757,-1.,1.97516705321494));
#21193=CARTESIAN_POINT('Ctrl Pts',(0.75983714745219,-1.,1.98143741418172));
#21194=CARTESIAN_POINT('Ctrl Pts',(0.759080037802488,-1.,1.98771456680874));
#21195=CARTESIAN_POINT('Ctrl Pts',(0.758281796766761,-1.,1.99399831098817));
#21196=CARTESIAN_POINT('Ctrl Pts',(0.757442676862724,-1.,2.00028834739178));
#21197=CARTESIAN_POINT('Ctrl Pts',(0.75656290464667,-1.,2.0065843158773));
#21198=CARTESIAN_POINT('Ctrl Pts',(0.755642704957865,-1.,2.01288584328084));
#21199=CARTESIAN_POINT('Ctrl Pts',(0.754682330722816,-1.,2.01919259405809));
#21200=CARTESIAN_POINT('Ctrl Pts',(0.753682061112768,-1.,2.02550428623313));
#21201=CARTESIAN_POINT('Ctrl Pts',(0.75264218048721,-1.,2.03182068456221));
#21202=CARTESIAN_POINT('Ctrl Pts',(0.751562963361115,-1.,2.03814160092099));
#21203=CARTESIAN_POINT('Ctrl Pts',(0.750444657875575,-1.,2.04446689147979));
#21204=CARTESIAN_POINT('Ctrl Pts',(0.749287468665046,-1.,2.05079645592154));
#21205=CARTESIAN_POINT('Ctrl Pts',(0.748091554183802,-1.,2.05713023031007));
#21206=CARTESIAN_POINT('Ctrl Pts',(0.747103932787919,-1.,2.06220058927826));
#21207=CARTESIAN_POINT('Ctrl Pts',(0.7463458715442,-1.,2.06600523016815));
#21208=CARTESIAN_POINT('Ctrl Pts',(0.745832791378367,-1.,2.06854248895728));
#21209=CARTESIAN_POINT('Ctrl Pts',(0.7455743247944,-1.,2.0698113262342));
#21210=CARTESIAN_POINT('',(0.61342227326009,-1.,2.11275013067528));
#21211=CARTESIAN_POINT('',(0.7455743247944,-1.,2.0698113262342));
#21212=CARTESIAN_POINT('',(0.383122945602004,-1.,1.7075470150345));
#21213=CARTESIAN_POINT('Ctrl Pts',(0.61342227326009,-1.,2.11275013067528));
#21214=CARTESIAN_POINT('Ctrl Pts',(0.6124673655618,-1.,2.11187554259986));
#21215=CARTESIAN_POINT('Ctrl Pts',(0.610560911689898,-1.,2.11012443807238));
#21216=CARTESIAN_POINT('Ctrl Pts',(0.607711315454876,-1.,2.1074919961518));
#21217=CARTESIAN_POINT('Ctrl Pts',(0.60393203073603,-1.,2.10397049886949));
#21218=CARTESIAN_POINT('Ctrl Pts',(0.599241616420533,-1.,2.0995493086477));
#21219=CARTESIAN_POINT('Ctrl Pts',(0.594585006052162,-1.,2.0951087622027));
#21220=CARTESIAN_POINT('Ctrl Pts',(0.589962365403406,-1.,2.09064881812129));
#21221=CARTESIAN_POINT('Ctrl Pts',(0.585373918991617,-1.,2.08616943727951));
#21222=CARTESIAN_POINT('Ctrl Pts',(0.580819952108063,-1.,2.08167059018418));
#21223=CARTESIAN_POINT('Ctrl Pts',(0.576300797416844,-1.,2.07715226767559));
#21224=CARTESIAN_POINT('Ctrl Pts',(0.571816823242602,-1.,2.07261449292824));
#21225=CARTESIAN_POINT('Ctrl Pts',(0.567368421181087,-1.,2.06805732997334));
#21226=CARTESIAN_POINT('Ctrl Pts',(0.562955993082261,-1.,2.06348090160589));
#21227=CARTESIAN_POINT('Ctrl Pts',(0.558579940185151,-1.,2.05888537756462));
#21228=CARTESIAN_POINT('Ctrl Pts',(0.554240657463906,-1.,2.05427091604413));
#21229=CARTESIAN_POINT('Ctrl Pts',(0.549938525150295,-1.,2.04963761077958));
#21230=CARTESIAN_POINT('Ctrl Pts',(0.54567390381743,-1.,2.04498544714588));
#21231=CARTESIAN_POINT('Ctrl Pts',(0.541447120615659,-1.,2.04031422690527));
#21232=CARTESIAN_POINT('Ctrl Pts',(0.537258489833262,-1.,2.03562362954037));
#21233=CARTESIAN_POINT('Ctrl Pts',(0.533108355132976,-1.,2.03091336214426));
#21234=CARTESIAN_POINT('Ctrl Pts',(0.528997127241914,-1.,2.0261832908329));
#21235=CARTESIAN_POINT('Ctrl Pts',(0.524925318333476,-1.,2.02143356304698));
#21236=CARTESIAN_POINT('Ctrl Pts',(0.52089359039937,-1.,2.01666477917286));
#21237=CARTESIAN_POINT('Ctrl Pts',(0.516902681728687,-1.,2.01187773939242));
#21238=CARTESIAN_POINT('Ctrl Pts',(0.512953306961792,-1.,2.00707309946949));
#21239=CARTESIAN_POINT('Ctrl Pts',(0.509046069886157,-1.,2.00225107134734));
#21240=CARTESIAN_POINT('Ctrl Pts',(0.505181361323026,-1.,1.99741107463572));
#21241=CARTESIAN_POINT('Ctrl Pts',(0.501359287727146,-1.,1.99255149126155));
#21242=CARTESIAN_POINT('Ctrl Pts',(0.497579909545574,-1.,1.98767044752932));
#21243=CARTESIAN_POINT('Ctrl Pts',(0.493843476541494,-1.,1.98276658761821));
#21244=CARTESIAN_POINT('Ctrl Pts',(0.490150627860952,-1.,1.97783973019229));
#21245=CARTESIAN_POINT('Ctrl Pts',(0.486502692907658,-1.,1.97289186263272));
#21246=CARTESIAN_POINT('Ctrl Pts',(0.48290166212069,-1.,1.96792703422362));
#21247=CARTESIAN_POINT('Ctrl Pts',(0.479349583074855,-1.,1.96294933055943));
#21248=CARTESIAN_POINT('Ctrl Pts',(0.475848034683176,-1.,1.95796111148177));
#21249=CARTESIAN_POINT('Ctrl Pts',(0.472397672264072,-1.,1.95296148278133));
#21250=CARTESIAN_POINT('Ctrl Pts',(0.468997482913135,-1.,1.94794381136514));
#21251=CARTESIAN_POINT('Ctrl Pts',(0.46564546202603,-1.,1.9428979419619));
#21252=CARTESIAN_POINT('Ctrl Pts',(0.462340031009056,-1.,1.93781486640821));
#21253=CARTESIAN_POINT('Ctrl Pts',(0.459081234547926,-1.,1.93269066517934));
#21254=CARTESIAN_POINT('Ctrl Pts',(0.45587200517437,-1.,1.92753067150476));
#21255=CARTESIAN_POINT('Ctrl Pts',(0.452719478359432,-1.,1.92235380648502));
#21256=CARTESIAN_POINT('Ctrl Pts',(0.449632260106662,-1.,1.91718342555755));
#21257=CARTESIAN_POINT('Ctrl Pts',(0.446617343485711,-1.,1.9120369998112));
#21258=CARTESIAN_POINT('Ctrl Pts',(0.44367755684915,-1.,1.90691756144898));
#21259=CARTESIAN_POINT('Ctrl Pts',(0.440807833704038,-1.,1.90180124389086));
#21260=CARTESIAN_POINT('Ctrl Pts',(0.437995003948244,-1.,1.89663648956466));
#21261=CARTESIAN_POINT('Ctrl Pts',(0.435225660963383,-1.,1.89136993975504));
#21262=CARTESIAN_POINT('Ctrl Pts',(0.432493038548748,-1.,1.88596913666793));
#21263=CARTESIAN_POINT('Ctrl Pts',(0.429803062482344,-1.,1.88044229001832));
#21264=CARTESIAN_POINT('Ctrl Pts',(0.427183828519102,-1.,1.87486989291484));
#21265=CARTESIAN_POINT('Ctrl Pts',(0.424678177291358,-1.,1.86937803944323));
#21266=CARTESIAN_POINT('Ctrl Pts',(0.422327307418275,-1.,1.86408083334028));
#21267=CARTESIAN_POINT('Ctrl Pts',(0.420157287975619,-1.,1.85903281096686));
#21268=CARTESIAN_POINT('Ctrl Pts',(0.418164129143534,-1.,1.85417632856234));
#21269=CARTESIAN_POINT('Ctrl Pts',(0.416300022038864,-1.,1.84929312929882));
#21270=CARTESIAN_POINT('Ctrl Pts',(0.41448743825434,-1.,1.8440575707371));
#21271=CARTESIAN_POINT('Ctrl Pts',(0.412633125322161,-1.,1.83808953475839));
#21272=CARTESIAN_POINT('Ctrl Pts',(0.410641256301674,-1.,1.83100408895216));
#21273=CARTESIAN_POINT('Ctrl Pts',(0.408428948108533,-1.,1.8224702267854));
#21274=CARTESIAN_POINT('Ctrl Pts',(0.405933518411838,-1.,1.81223801813988));
#21275=CARTESIAN_POINT('Ctrl Pts',(0.403107976170441,-1.,1.80012077176221));
#21276=CARTESIAN_POINT('Ctrl Pts',(0.39991940378308,-1.,1.78598826347533));
#21277=CARTESIAN_POINT('Ctrl Pts',(0.39634619612042,-1.,1.7697556004756));
#21278=CARTESIAN_POINT('Ctrl Pts',(0.392375812294307,-1.,1.75137405313962));
#21279=CARTESIAN_POINT('Ctrl Pts',(0.388877023509191,-1.,1.7349317097561));
#21280=CARTESIAN_POINT('Ctrl Pts',(0.38607079032701,-1.,1.72162022246158));
#21281=CARTESIAN_POINT('Ctrl Pts',(0.384119047315541,-1.,1.71231062891958));
#21282=CARTESIAN_POINT('Ctrl Pts',(0.383122945602004,-1.,1.7075470150345));
#21283=CARTESIAN_POINT('',(0.163289472382896,-1.,1.74236521665491));
#21284=CARTESIAN_POINT('Origin',(0.,-1.,0.));
#21285=CARTESIAN_POINT('',(0.0694764450219578,-1.,2.19890268624765));
#21286=CARTESIAN_POINT('Ctrl Pts',(0.163289472382896,-1.,1.74236521665491));
#21287=CARTESIAN_POINT('Ctrl Pts',(0.163814161002002,-1.,1.7472034950333));
#21288=CARTESIAN_POINT('Ctrl Pts',(0.164834765707158,-1.,1.75666056638427));
#21289=CARTESIAN_POINT('Ctrl Pts',(0.1662793551464,-1.,1.77018771684844));
#21290=CARTESIAN_POINT('Ctrl Pts',(0.168032772805197,-1.,1.7869064998507));
#21291=CARTESIAN_POINT('Ctrl Pts',(0.169936923904608,-1.,1.80561530629706));
#21292=CARTESIAN_POINT('Ctrl Pts',(0.171554770204119,-1.,1.82215766811545));
#21293=CARTESIAN_POINT('Ctrl Pts',(0.1728894428919,-1.,1.83658380527692));
#21294=CARTESIAN_POINT('Ctrl Pts',(0.173946627587731,-1.,1.8489811319852));
#21295=CARTESIAN_POINT('Ctrl Pts',(0.17473525927603,-1.,1.85948367088837));
#21296=CARTESIAN_POINT('Ctrl Pts',(0.175268337590757,-1.,1.86828349694799));
#21297=CARTESIAN_POINT('Ctrl Pts',(0.175563480746485,-1.,1.87563767773588));
#21298=CARTESIAN_POINT('Ctrl Pts',(0.175644148889698,-1.,1.88188663145367));
#21299=CARTESIAN_POINT('Ctrl Pts',(0.175538155840648,-1.,1.88742606273259));
#21300=CARTESIAN_POINT('Ctrl Pts',(0.175274276190844,-1.,1.892646301985));
#21301=CARTESIAN_POINT('Ctrl Pts',(0.174879405091263,-1.,1.89788101117132));
#21302=CARTESIAN_POINT('Ctrl Pts',(0.174375518661085,-1.,1.90335253862834));
#21303=CARTESIAN_POINT('Ctrl Pts',(0.173776635257816,-1.,1.90911693975267));
#21304=CARTESIAN_POINT('Ctrl Pts',(0.173090695383496,-1.,1.91511429159527));
#21305=CARTESIAN_POINT('Ctrl Pts',(0.172321621259513,-1.,1.9212233439798));
#21306=CARTESIAN_POINT('Ctrl Pts',(0.171471191532988,-1.,1.92731093582036));
#21307=CARTESIAN_POINT('Ctrl Pts',(0.170541253116201,-1.,1.93329183155539));
#21308=CARTESIAN_POINT('Ctrl Pts',(0.16953490481749,-1.,1.93915639211581));
#21309=CARTESIAN_POINT('Ctrl Pts',(0.168455741607556,-1.,1.94493757756931));
#21310=CARTESIAN_POINT('Ctrl Pts',(0.167307501784475,-1.,1.95069027794294));
#21311=CARTESIAN_POINT('Ctrl Pts',(0.166093592002812,-1.,1.9564675971873));
#21312=CARTESIAN_POINT('Ctrl Pts',(0.164816568920269,-1.,1.96229379940136));
#21313=CARTESIAN_POINT('Ctrl Pts',(0.163478185457734,-1.,1.96816512677967));
#21314=CARTESIAN_POINT('Ctrl Pts',(0.162079693556288,-1.,1.97406280235188));
#21315=CARTESIAN_POINT('Ctrl Pts',(0.160622060784611,-1.,1.97996195437559));
#21316=CARTESIAN_POINT('Ctrl Pts',(0.159106226437299,-1.,1.98584238283292));
#21317=CARTESIAN_POINT('Ctrl Pts',(0.157533331459227,-1.,1.99169810931908));
#21318=CARTESIAN_POINT('Ctrl Pts',(0.155904629548783,-1.,1.99753284771497));
#21319=CARTESIAN_POINT('Ctrl Pts',(0.154221403049722,-1.,2.00335565310543));
#21320=CARTESIAN_POINT('Ctrl Pts',(0.152484883621449,-1.,2.00917680318424));
#21321=CARTESIAN_POINT('Ctrl Pts',(0.150696157673078,-1.,2.01500291940238));
#21322=CARTESIAN_POINT('Ctrl Pts',(0.148856124775337,-1.,2.02083464969894));
#21323=CARTESIAN_POINT('Ctrl Pts',(0.146965557332583,-1.,2.02666926182017));
#21324=CARTESIAN_POINT('Ctrl Pts',(0.145025140186057,-1.,2.03250223739942));
#21325=CARTESIAN_POINT('Ctrl Pts',(0.143035515058208,-1.,2.03832911025912));
#21326=CARTESIAN_POINT('Ctrl Pts',(0.140997332152546,-1.,2.04414757947916));
#21327=CARTESIAN_POINT('Ctrl Pts',(0.138911255368966,-1.,2.04995762001328));
#21328=CARTESIAN_POINT('Ctrl Pts',(0.136777941218043,-1.,2.05576044414264));
#21329=CARTESIAN_POINT('Ctrl Pts',(0.134598026192106,-1.,2.06155781517842));
#21330=CARTESIAN_POINT('Ctrl Pts',(0.13237211154771,-1.,2.06735123910326));
#21331=CARTESIAN_POINT('Ctrl Pts',(0.130100748328403,-1.,2.07314114713063));
#21332=CARTESIAN_POINT('Ctrl Pts',(0.12778444527612,-1.,2.07892715110987));
#21333=CARTESIAN_POINT('Ctrl Pts',(0.125423679412061,-1.,2.08470840653643));
#21334=CARTESIAN_POINT('Ctrl Pts',(0.123018905621083,-1.,2.09048392424825));
#21335=CARTESIAN_POINT('Ctrl Pts',(0.120570567965122,-1.,2.0962529286773));
#21336=CARTESIAN_POINT('Ctrl Pts',(0.118079107988355,-1.,2.102015121329));
#21337=CARTESIAN_POINT('Ctrl Pts',(0.115544957687926,-1.,2.10777050261309));
#21338=CARTESIAN_POINT('Ctrl Pts',(0.112968534419737,-1.,2.11351924490306));
#21339=CARTESIAN_POINT('Ctrl Pts',(0.110350236135025,-1.,2.11926155590865));
#21340=CARTESIAN_POINT('Ctrl Pts',(0.10769043523109,-1.,2.12499752307));
#21341=CARTESIAN_POINT('Ctrl Pts',(0.104989479152739,-1.,2.13072704887293));
#21342=CARTESIAN_POINT('Ctrl Pts',(0.1022477005561,-1.,2.13644992667165));
#21343=CARTESIAN_POINT('Ctrl Pts',(0.0994654261990913,-1.,2.14216588396025));
#21344=CARTESIAN_POINT('Ctrl Pts',(0.0966429852305456,-1.,2.14787463531795));
#21345=CARTESIAN_POINT('Ctrl Pts',(0.0937807218867641,-1.,2.1535759397817));
#21346=CARTESIAN_POINT('Ctrl Pts',(0.0908789888107263,-1.,2.15926961544516));
#21347=CARTESIAN_POINT('Ctrl Pts',(0.087938129138692,-1.,2.16495552645014));
#21348=CARTESIAN_POINT('Ctrl Pts',(0.084958462083537,-1.,2.17063357870952));
#21349=CARTESIAN_POINT('Ctrl Pts',(0.0819402680872763,-1.,2.176303712113));
#21350=CARTESIAN_POINT('Ctrl Pts',(0.078883772768524,-1.,2.18196589448887));
#21351=CARTESIAN_POINT('Ctrl Pts',(0.0757891465836145,-1.,2.1876201139953));
#21352=CARTESIAN_POINT('Ctrl Pts',(0.0732830357306722,-1.,2.19213712013662));
#21353=CARTESIAN_POINT('Ctrl Pts',(0.0713863779526151,-1.,2.19552129484002));
#21354=CARTESIAN_POINT('Ctrl Pts',(0.0701143536325487,-1.,2.19777582085423));
#21355=CARTESIAN_POINT('Ctrl Pts',(0.0694764450219578,-1.,2.19890268624765));
#21356=CARTESIAN_POINT('',(-0.0694764450219586,-1.,2.19890268624765));
#21357=CARTESIAN_POINT('',(0.0694764450219578,-1.,2.19890268624765));
#21358=CARTESIAN_POINT('',(-0.163289472382896,-1.,1.74236521665491));
#21359=CARTESIAN_POINT('Ctrl Pts',(-0.0694764450219586,-1.,2.19890268624765));
#21360=CARTESIAN_POINT('Ctrl Pts',(-0.0701143536324929,-1.,2.19777582085261));
#21361=CARTESIAN_POINT('Ctrl Pts',(-0.071386377952463,-1.,2.19552129483562));
#21362=CARTESIAN_POINT('Ctrl Pts',(-0.0732830357304279,-1.,2.19213712012956));
#21363=CARTESIAN_POINT('Ctrl Pts',(-0.0757891465833414,-1.,2.1876201139874));
#21364=CARTESIAN_POINT('Ctrl Pts',(-0.078883772768323,-1.,2.18196589448304));
#21365=CARTESIAN_POINT('Ctrl Pts',(-0.0819402680871942,-1.,2.1763037121106));
#21366=CARTESIAN_POINT('Ctrl Pts',(-0.0849584620835646,-1.,2.17063357871031));
#21367=CARTESIAN_POINT('Ctrl Pts',(-0.0879381291387825,-1.,2.16495552645275));
#21368=CARTESIAN_POINT('Ctrl Pts',(-0.0908789888108269,-1.,2.15926961544808));
#21369=CARTESIAN_POINT('Ctrl Pts',(-0.0937807218868348,-1.,2.15357593978377));
#21370=CARTESIAN_POINT('Ctrl Pts',(-0.0966429852305691,-1.,2.14787463531864));
#21371=CARTESIAN_POINT('Ctrl Pts',(-0.0994654261990745,-1.,2.14216588395974));
#21372=CARTESIAN_POINT('Ctrl Pts',(-0.102247700556064,-1.,2.13644992667052));
#21373=CARTESIAN_POINT('Ctrl Pts',(-0.104989479152703,-1.,2.1307270488718));
#21374=CARTESIAN_POINT('Ctrl Pts',(-0.107690435231068,-1.,2.12499752306927));
#21375=CARTESIAN_POINT('Ctrl Pts',(-0.11035023613502,-1.,2.11926155590849));
#21376=CARTESIAN_POINT('Ctrl Pts',(-0.112968534419746,-1.,2.11351924490335));
#21377=CARTESIAN_POINT('Ctrl Pts',(-0.115544957687941,-1.,2.10777050261359));
#21378=CARTESIAN_POINT('Ctrl Pts',(-0.118079107988368,-1.,2.10201512132945));
#21379=CARTESIAN_POINT('Ctrl Pts',(-0.120570567965129,-1.,2.09625292867756));
#21380=CARTESIAN_POINT('Ctrl Pts',(-0.123018905621083,-1.,2.09048392424826));
#21381=CARTESIAN_POINT('Ctrl Pts',(-0.125423679412058,-1.,2.08470840653628));
#21382=CARTESIAN_POINT('Ctrl Pts',(-0.127784445276116,-1.,2.07892715110967));
#21383=CARTESIAN_POINT('Ctrl Pts',(-0.130100748328401,-1.,2.07314114713047));
#21384=CARTESIAN_POINT('Ctrl Pts',(-0.13237211154771,-1.,2.06735123910319));
#21385=CARTESIAN_POINT('Ctrl Pts',(-0.134598026192107,-1.,2.06155781517844));
#21386=CARTESIAN_POINT('Ctrl Pts',(-0.136777941218044,-1.,2.0557604441427));
#21387=CARTESIAN_POINT('Ctrl Pts',(-0.138911255368966,-1.,2.04995762001333));
#21388=CARTESIAN_POINT('Ctrl Pts',(-0.140997332152546,-1.,2.04414757947919));
#21389=CARTESIAN_POINT('Ctrl Pts',(-0.143035515058208,-1.,2.03832911025913));
#21390=CARTESIAN_POINT('Ctrl Pts',(-0.145025140186058,-1.,2.03250223739941));
#21391=CARTESIAN_POINT('Ctrl Pts',(-0.146965557332586,-1.,2.02666926182017));
#21392=CARTESIAN_POINT('Ctrl Pts',(-0.148856124775343,-1.,2.02083464969897));
#21393=CARTESIAN_POINT('Ctrl Pts',(-0.150696157673084,-1.,2.01500291940243));
#21394=CARTESIAN_POINT('Ctrl Pts',(-0.152484883621452,-1.,2.00917680318426));
#21395=CARTESIAN_POINT('Ctrl Pts',(-0.154221403049719,-1.,2.00335565310539));
#21396=CARTESIAN_POINT('Ctrl Pts',(-0.155904629548775,-1.,1.99753284771487));
#21397=CARTESIAN_POINT('Ctrl Pts',(-0.157533331459215,-1.,1.99169810931893));
#21398=CARTESIAN_POINT('Ctrl Pts',(-0.159106226437289,-1.,1.98584238283279));
#21399=CARTESIAN_POINT('Ctrl Pts',(-0.16062206078461,-1.,1.97996195437557));
#21400=CARTESIAN_POINT('Ctrl Pts',(-0.162079693556302,-1.,1.97406280235204));
#21401=CARTESIAN_POINT('Ctrl Pts',(-0.16347818545776,-1.,1.96816512678));
#21402=CARTESIAN_POINT('Ctrl Pts',(-0.1648165689203,-1.,1.96229379940174));
#21403=CARTESIAN_POINT('Ctrl Pts',(-0.166093592002833,-1.,1.95646759718755));
#21404=CARTESIAN_POINT('Ctrl Pts',(-0.167307501784469,-1.,1.95069027794286));
#21405=CARTESIAN_POINT('Ctrl Pts',(-0.168455741607516,-1.,1.94493757756879));
#21406=CARTESIAN_POINT('Ctrl Pts',(-0.169534904817425,-1.,1.93915639211497));
#21407=CARTESIAN_POINT('Ctrl Pts',(-0.170541253116136,-1.,1.93329183155455));
#21408=CARTESIAN_POINT('Ctrl Pts',(-0.17147119153296,-1.,1.92731093582));
#21409=CARTESIAN_POINT('Ctrl Pts',(-0.172321621259557,-1.,1.92122334398034));
#21410=CARTESIAN_POINT('Ctrl Pts',(-0.173090695383619,-1.,1.91511429159681));
#21411=CARTESIAN_POINT('Ctrl Pts',(-0.173776635257984,-1.,1.90911693975475));
#21412=CARTESIAN_POINT('Ctrl Pts',(-0.174375518661222,-1.,1.90335253863003));
#21413=CARTESIAN_POINT('Ctrl Pts',(-0.174879405091277,-1.,1.89788101117148));
#21414=CARTESIAN_POINT('Ctrl Pts',(-0.175274276190664,-1.,1.89264630198279));
#21415=CARTESIAN_POINT('Ctrl Pts',(-0.175538155840286,-1.,1.88742606272818));
#21416=CARTESIAN_POINT('Ctrl Pts',(-0.175644148889271,-1.,1.88188663144846));
#21417=CARTESIAN_POINT('Ctrl Pts',(-0.175563480746206,-1.,1.87563767773249));
#21418=CARTESIAN_POINT('Ctrl Pts',(-0.175268337590901,-1.,1.86828349694972));
#21419=CARTESIAN_POINT('Ctrl Pts',(-0.174735259276856,-1.,1.85948367089838));
#21420=CARTESIAN_POINT('Ctrl Pts',(-0.173946627589401,-1.,1.84898113200543));
#21421=CARTESIAN_POINT('Ctrl Pts',(-0.17288944289442,-1.,1.83658380530747));
#21422=CARTESIAN_POINT('Ctrl Pts',(-0.171554770207306,-1.,1.82215766815414));
#21423=CARTESIAN_POINT('Ctrl Pts',(-0.169936923908078,-1.,1.80561530633924));
#21424=CARTESIAN_POINT('Ctrl Pts',(-0.16803277280837,-1.,1.78690649988931));
#21425=CARTESIAN_POINT('Ctrl Pts',(-0.166279355148738,-1.,1.77018771687692));
#21426=CARTESIAN_POINT('Ctrl Pts',(-0.164834765708484,-1.,1.75666056640041));
#21427=CARTESIAN_POINT('Ctrl Pts',(-0.163814161002474,-1.,1.74720349503904));
#21428=CARTESIAN_POINT('Ctrl Pts',(-0.163289472382896,-1.,1.74236521665491));
#21429=CARTESIAN_POINT('',(-0.383122945602004,-1.,1.7075470150345));
#21430=CARTESIAN_POINT('Origin',(0.,-1.,0.));
#21431=CARTESIAN_POINT('',(-0.61342227326009,-1.,2.11275013067528));
#21432=CARTESIAN_POINT('Ctrl Pts',(-0.383122945602004,-1.,1.7075470150345));
#21433=CARTESIAN_POINT('Ctrl Pts',(-0.384119047314215,-1.,1.71231062891398));
#21434=CARTESIAN_POINT('Ctrl Pts',(-0.386070790323281,-1.,1.72162022244582));
#21435=CARTESIAN_POINT('Ctrl Pts',(-0.388877023502615,-1.,1.73493170972829));
#21436=CARTESIAN_POINT('Ctrl Pts',(-0.392375812285395,-1.,1.75137405310193));
#21437=CARTESIAN_POINT('Ctrl Pts',(-0.396346196110688,-1.,1.76975560043442));
#21438=CARTESIAN_POINT('Ctrl Pts',(-0.399919403774155,-1.,1.78598826343754));
#21439=CARTESIAN_POINT('Ctrl Pts',(-0.403107976163396,-1.,1.80012077173238));
#21440=CARTESIAN_POINT('Ctrl Pts',(-0.405933518407175,-1.,1.81223801812013));
#21441=CARTESIAN_POINT('Ctrl Pts',(-0.408428948106227,-1.,1.82247022677562));
#21442=CARTESIAN_POINT('Ctrl Pts',(-0.410641256301276,-1.,1.83100408895047));
#21443=CARTESIAN_POINT('Ctrl Pts',(-0.412633125322945,-1.,1.8380895347617));
#21444=CARTESIAN_POINT('Ctrl Pts',(-0.414487438255542,-1.,1.84405757074218));
#21445=CARTESIAN_POINT('Ctrl Pts',(-0.416300022039885,-1.,1.84929312930314));
#21446=CARTESIAN_POINT('Ctrl Pts',(-0.418164129144045,-1.,1.8541763285645));
#21447=CARTESIAN_POINT('Ctrl Pts',(-0.420157287975583,-1.,1.8590328109667));
#21448=CARTESIAN_POINT('Ctrl Pts',(-0.422327307417885,-1.,1.86408083333863));
#21449=CARTESIAN_POINT('Ctrl Pts',(-0.424678177290876,-1.,1.8693780394412));
#21450=CARTESIAN_POINT('Ctrl Pts',(-0.427183828518743,-1.,1.87486989291333));
#21451=CARTESIAN_POINT('Ctrl Pts',(-0.429803062482217,-1.,1.88044229001778));
#21452=CARTESIAN_POINT('Ctrl Pts',(-0.432493038548833,-1.,1.88596913666828));
#21453=CARTESIAN_POINT('Ctrl Pts',(-0.43522566096358,-1.,1.89136993975585));
#21454=CARTESIAN_POINT('Ctrl Pts',(-0.437995003948443,-1.,1.89663648956549));
#21455=CARTESIAN_POINT('Ctrl Pts',(-0.440807833704161,-1.,1.90180124389137));
#21456=CARTESIAN_POINT('Ctrl Pts',(-0.44367755684917,-1.,1.90691756144906));
#21457=CARTESIAN_POINT('Ctrl Pts',(-0.446617343485651,-1.,1.91203699981095));
#21458=CARTESIAN_POINT('Ctrl Pts',(-0.449632260106572,-1.,1.91718342555717));
#21459=CARTESIAN_POINT('Ctrl Pts',(-0.452719478359356,-1.,1.9223538064847));
#21460=CARTESIAN_POINT('Ctrl Pts',(-0.455872005174335,-1.,1.92753067150461));
#21461=CARTESIAN_POINT('Ctrl Pts',(-0.459081234547931,-1.,1.93269066517936));
#21462=CARTESIAN_POINT('Ctrl Pts',(-0.462340031009087,-1.,1.93781486640834));
#21463=CARTESIAN_POINT('Ctrl Pts',(-0.465645462026065,-1.,1.94289794196205));
#21464=CARTESIAN_POINT('Ctrl Pts',(-0.468997482913158,-1.,1.94794381136524));
#21465=CARTESIAN_POINT('Ctrl Pts',(-0.47239767226408,-1.,1.95296148278136));
#21466=CARTESIAN_POINT('Ctrl Pts',(-0.475848034683172,-1.,1.95796111148175));
#21467=CARTESIAN_POINT('Ctrl Pts',(-0.479349583074846,-1.,1.96294933055938));
#21468=CARTESIAN_POINT('Ctrl Pts',(-0.482901662120687,-1.,1.96792703422358));
#21469=CARTESIAN_POINT('Ctrl Pts',(-0.486502692907661,-1.,1.97289186263272));
#21470=CARTESIAN_POINT('Ctrl Pts',(-0.490150627860955,-1.,1.97783973019229));
#21471=CARTESIAN_POINT('Ctrl Pts',(-0.493843476541492,-1.,1.9827665876182));
#21472=CARTESIAN_POINT('Ctrl Pts',(-0.497579909545564,-1.,1.98767044752929));
#21473=CARTESIAN_POINT('Ctrl Pts',(-0.501359287727129,-1.,1.9925514912615));
#21474=CARTESIAN_POINT('Ctrl Pts',(-0.505181361323011,-1.,1.99741107463567));
#21475=CARTESIAN_POINT('Ctrl Pts',(-0.509046069886152,-1.,2.00225107134733));
#21476=CARTESIAN_POINT('Ctrl Pts',(-0.512953306961814,-1.,2.00707309946955));
#21477=CARTESIAN_POINT('Ctrl Pts',(-0.516902681728733,-1.,2.01187773939257));
#21478=CARTESIAN_POINT('Ctrl Pts',(-0.520893590399428,-1.,2.01666477917305));
#21479=CARTESIAN_POINT('Ctrl Pts',(-0.524925318333518,-1.,2.02143356304712));
#21480=CARTESIAN_POINT('Ctrl Pts',(-0.528997127241911,-1.,2.02618329083289));
#21481=CARTESIAN_POINT('Ctrl Pts',(-0.533108355132905,-1.,2.03091336214401));
#21482=CARTESIAN_POINT('Ctrl Pts',(-0.537258489833134,-1.,2.03562362953993));
#21483=CARTESIAN_POINT('Ctrl Pts',(-0.54144712061552,-1.,2.0403142269048));
#21484=CARTESIAN_POINT('Ctrl Pts',(-0.545673903817348,-1.,2.0449854471456));
#21485=CARTESIAN_POINT('Ctrl Pts',(-0.549938525150342,-1.,2.04963761077974));
#21486=CARTESIAN_POINT('Ctrl Pts',(-0.55424065746411,-1.,2.05427091604482));
#21487=CARTESIAN_POINT('Ctrl Pts',(-0.558579940185467,-1.,2.05888537756571));
#21488=CARTESIAN_POINT('Ctrl Pts',(-0.562955993082574,-1.,2.06348090160697));
#21489=CARTESIAN_POINT('Ctrl Pts',(-0.567368421181229,-1.,2.06805732997383));
#21490=CARTESIAN_POINT('Ctrl Pts',(-0.571816823242411,-1.,2.07261449292757));
#21491=CARTESIAN_POINT('Ctrl Pts',(-0.576300797416275,-1.,2.07715226767361));
#21492=CARTESIAN_POINT('Ctrl Pts',(-0.580819952107257,-1.,2.08167059018138));
#21493=CARTESIAN_POINT('Ctrl Pts',(-0.585373918990895,-1.,2.086169437277));
#21494=CARTESIAN_POINT('Ctrl Pts',(-0.589962365403189,-1.,2.09064881812053));
#21495=CARTESIAN_POINT('Ctrl Pts',(-0.594585006052824,-1.,2.09510876220501));
#21496=CARTESIAN_POINT('Ctrl Pts',(-0.599241616422144,-1.,2.09954930865331));
#21497=CARTESIAN_POINT('Ctrl Pts',(-0.603932030738212,-1.,2.10397049887709));
#21498=CARTESIAN_POINT('Ctrl Pts',(-0.607711315456826,-1.,2.10749199615859));
#21499=CARTESIAN_POINT('Ctrl Pts',(-0.610560911691113,-1.,2.11012443807661));
#21500=CARTESIAN_POINT('Ctrl Pts',(-0.61246736556225,-1.,2.11187554260142));
#21501=CARTESIAN_POINT('Ctrl Pts',(-0.61342227326009,-1.,2.11275013067528));
#21502=CARTESIAN_POINT('',(-0.745574324794401,-1.,2.0698113262342));
#21503=CARTESIAN_POINT('',(-0.61342227326009,-1.,2.11275013067528));
#21504=CARTESIAN_POINT('',(-0.693717979106306,-1.,1.60662857109684));
#21505=CARTESIAN_POINT('Ctrl Pts',(-0.745574324794401,-1.,2.0698113262342));
#21506=CARTESIAN_POINT('Ctrl Pts',(-0.74583279137781,-1.,2.06854248895575));
#21507=CARTESIAN_POINT('Ctrl Pts',(-0.746345871542696,-1.,2.06600523016401));
#21508=CARTESIAN_POINT('Ctrl Pts',(-0.747103932785504,-1.,2.06220058927162));
#21509=CARTESIAN_POINT('Ctrl Pts',(-0.748091554181101,-1.,2.05713023030263));
#21510=CARTESIAN_POINT('Ctrl Pts',(-0.749287468663053,-1.,2.05079645591606));
#21511=CARTESIAN_POINT('Ctrl Pts',(-0.750444657874758,-1.,2.04446689147754));
#21512=CARTESIAN_POINT('Ctrl Pts',(-0.751562963361384,-1.,2.03814160092173));
#21513=CARTESIAN_POINT('Ctrl Pts',(-0.752642180488104,-1.,2.03182068456467));
#21514=CARTESIAN_POINT('Ctrl Pts',(-0.753682061113766,-1.,2.02550428623587));
#21515=CARTESIAN_POINT('Ctrl Pts',(-0.75468233072352,-1.,2.01919259406003));
#21516=CARTESIAN_POINT('Ctrl Pts',(-0.7556427049581,-1.,2.01288584328149));
#21517=CARTESIAN_POINT('Ctrl Pts',(-0.756562904646496,-1.,2.00658431587682));
#21518=CARTESIAN_POINT('Ctrl Pts',(-0.757442676862341,-1.,2.00028834739072));
#21519=CARTESIAN_POINT('Ctrl Pts',(-0.758281796766377,-1.,1.9939983109871));
#21520=CARTESIAN_POINT('Ctrl Pts',(-0.759080037802243,-1.,1.98771456680806));
#21521=CARTESIAN_POINT('Ctrl Pts',(-0.759837147452135,-1.,1.98143741418156));
#21522=CARTESIAN_POINT('Ctrl Pts',(-0.760552825409855,-1.,1.97516705321521));
#21523=CARTESIAN_POINT('Ctrl Pts',(-0.761226690483986,-1.,1.96890351582545));
#21524=CARTESIAN_POINT('Ctrl Pts',(-0.761858300014575,-1.,1.96264672744229));
#21525=CARTESIAN_POINT('Ctrl Pts',(-0.762447203806263,-1.,1.95639665309893));
#21526=CARTESIAN_POINT('Ctrl Pts',(-0.762992990878774,-1.,1.95015342590025));
#21527=CARTESIAN_POINT('Ctrl Pts',(-0.76349533353858,-1.,1.94391746617626));
#21528=CARTESIAN_POINT('Ctrl Pts',(-0.763954049121393,-1.,1.93768964875867));
#21529=CARTESIAN_POINT('Ctrl Pts',(-0.764369010673889,-1.,1.93147105496367));
#21530=CARTESIAN_POINT('Ctrl Pts',(-0.764740025488189,-1.,1.92526263537041));
#21531=CARTESIAN_POINT('Ctrl Pts',(-0.765066729667095,-1.,1.91906491634197));
#21532=CARTESIAN_POINT('Ctrl Pts',(-0.765348465884739,-1.,1.91287765805174));
#21533=CARTESIAN_POINT('Ctrl Pts',(-0.765584196937936,-1.,1.90669961402362));
#21534=CARTESIAN_POINT('Ctrl Pts',(-0.765772772593395,-1.,1.90052930393599));
#21535=CARTESIAN_POINT('Ctrl Pts',(-0.765913193856979,-1.,1.89436577771389));
#21536=CARTESIAN_POINT('Ctrl Pts',(-0.76600483706209,-1.,1.88820926433409));
#21537=CARTESIAN_POINT('Ctrl Pts',(-0.766047794851869,-1.,1.88206215302561));
#21538=CARTESIAN_POINT('Ctrl Pts',(-0.766042837036759,-1.,1.87592888967886));
#21539=CARTESIAN_POINT('Ctrl Pts',(-0.765990708546111,-1.,1.86981398314345));
#21540=CARTESIAN_POINT('Ctrl Pts',(-0.765891519092557,-1.,1.86372027063314));
#21541=CARTESIAN_POINT('Ctrl Pts',(-0.765744212909305,-1.,1.85764741390391));
#21542=CARTESIAN_POINT('Ctrl Pts',(-0.765545710619023,-1.,1.85158945130054));
#21543=CARTESIAN_POINT('Ctrl Pts',(-0.765291664861971,-1.,1.8455369887591));
#21544=CARTESIAN_POINT('Ctrl Pts',(-0.764978057881687,-1.,1.83948181064823));
#21545=CARTESIAN_POINT('Ctrl Pts',(-0.764602549687845,-1.,1.8334207722714));
#21546=CARTESIAN_POINT('Ctrl Pts',(-0.764165902606055,-1.,1.8273599120008));
#21547=CARTESIAN_POINT('Ctrl Pts',(-0.763673465462854,-1.,1.82131873145297));
#21548=CARTESIAN_POINT('Ctrl Pts',(-0.763132003836783,-1.,1.81532118405566));
#21549=CARTESIAN_POINT('Ctrl Pts',(-0.762546129464036,-1.,1.80938551463989));
#21550=CARTESIAN_POINT('Ctrl Pts',(-0.761915336443516,-1.,1.80351583877334));
#21551=CARTESIAN_POINT('Ctrl Pts',(-0.761229695230359,-1.,1.79768986997735));
#21552=CARTESIAN_POINT('Ctrl Pts',(-0.760469555880425,-1.,1.79185815610802));
#21553=CARTESIAN_POINT('Ctrl Pts',(-0.759614401109868,-1.,1.78596964884526));
#21554=CARTESIAN_POINT('Ctrl Pts',(-0.75865062667738,-1.,1.77999411220912));
#21555=CARTESIAN_POINT('Ctrl Pts',(-0.757578264077238,-1.,1.77394167108342));
#21556=CARTESIAN_POINT('Ctrl Pts',(-0.756421896028403,-1.,1.76789396003141));
#21557=CARTESIAN_POINT('Ctrl Pts',(-0.755220979975262,-1.,1.7619781724032));
#21558=CARTESIAN_POINT('Ctrl Pts',(-0.75400925402848,-1.,1.75631083600175));
#21559=CARTESIAN_POINT('Ctrl Pts',(-0.752797683531377,-1.,1.75095139468809));
#21560=CARTESIAN_POINT('Ctrl Pts',(-0.751555614163629,-1.,1.74585086852298));
#21561=CARTESIAN_POINT('Ctrl Pts',(-0.75019343597954,-1.,1.74080458266705));
#21562=CARTESIAN_POINT('Ctrl Pts',(-0.748582462954855,-1.,1.73550351679848));
#21563=CARTESIAN_POINT('Ctrl Pts',(-0.746574710096436,-1.,1.72958533647399));
#21564=CARTESIAN_POINT('Ctrl Pts',(-0.744021445433764,-1.,1.7226822991693));
#21565=CARTESIAN_POINT('Ctrl Pts',(-0.740795162032088,-1.,1.71447789751927));
#21566=CARTESIAN_POINT('Ctrl Pts',(-0.736799665724771,-1.,1.70473309006121));
#21567=CARTESIAN_POINT('Ctrl Pts',(-0.731963238697195,-1.,1.69326921975743));
#21568=CARTESIAN_POINT('Ctrl Pts',(-0.726235967997433,-1.,1.67996158455503));
#21569=CARTESIAN_POINT('Ctrl Pts',(-0.719585433804282,-1.,1.6647288055568));
#21570=CARTESIAN_POINT('Ctrl Pts',(-0.711993139355394,-1.,1.64752408832016));
#21571=CARTESIAN_POINT('Ctrl Pts',(-0.705159151988319,-1.,1.63216541664676));
#21572=CARTESIAN_POINT('Ctrl Pts',(-0.699605146405088,-1.,1.61974673472612));
#21573=CARTESIAN_POINT('Ctrl Pts',(-0.695712097881194,-1.,1.61106790958151));
#21574=CARTESIAN_POINT('Ctrl Pts',(-0.693717979106306,-1.,1.60662857109684));
#21575=CARTESIAN_POINT('',(-0.892032620296855,-1.,1.5055822144029));
#21576=CARTESIAN_POINT('Origin',(0.,-1.,0.));
#21577=CARTESIAN_POINT('',(-1.23627494547115,-1.,1.81978687191668));
#21578=CARTESIAN_POINT('Ctrl Pts',(-0.892032620296855,-1.,1.5055822144029));
#21579=CARTESIAN_POINT('Ctrl Pts',(-0.894452006964543,-1.,1.50980486806688));
#21580=CARTESIAN_POINT('Ctrl Pts',(-0.899185047483511,-1.,1.51805569590094));
#21581=CARTESIAN_POINT('Ctrl Pts',(-0.905967409625651,-1.,1.52984849887993));
#21582=CARTESIAN_POINT('Ctrl Pts',(-0.914375919026456,-1.,1.54440491149498));
#21583=CARTESIAN_POINT('Ctrl Pts',(-0.923832188944341,-1.,1.56065988578893));
#21584=CARTESIAN_POINT('Ctrl Pts',(-0.932246680108685,-1.,1.57499388382243));
#21585=CARTESIAN_POINT('Ctrl Pts',(-0.939646377893399,-1.,1.58744937487176));
#21586=CARTESIAN_POINT('Ctrl Pts',(-0.946078063315257,-1.,1.59810042043673));
#21587=CARTESIAN_POINT('Ctrl Pts',(-0.951613284356035,-1.,1.60706069896936));
#21588=CARTESIAN_POINT('Ctrl Pts',(-0.956354422920671,-1.,1.61449324337085));
#21589=CARTESIAN_POINT('Ctrl Pts',(-0.960438326101729,-1.,1.62061638140221));
#21590=CARTESIAN_POINT('Ctrl Pts',(-0.964046107040536,-1.,1.62571930670187));
#21591=CARTESIAN_POINT('Ctrl Pts',(-0.967387853230345,-1.,1.63013849959461));
#21592=CARTESIAN_POINT('Ctrl Pts',(-0.970669715997509,-1.,1.63420665729798));
#21593=CARTESIAN_POINT('Ctrl Pts',(-0.974066058287418,-1.,1.63820952658144));
#21594=CARTESIAN_POINT('Ctrl Pts',(-0.977689794119416,-1.,1.64233990826687));
#21595=CARTESIAN_POINT('Ctrl Pts',(-0.981562530939489,-1.,1.64665139190656));
#21596=CARTESIAN_POINT('Ctrl Pts',(-0.985642622920821,-1.,1.65110016612638));
#21597=CARTESIAN_POINT('Ctrl Pts',(-0.989855627854165,-1.,1.65559044289699));
#21598=CARTESIAN_POINT('Ctrl Pts',(-0.994121836661306,-1.,1.66001553809947));
#21599=CARTESIAN_POINT('Ctrl Pts',(-0.998389654952758,-1.,1.66430758030376));
#21600=CARTESIAN_POINT('Ctrl Pts',(-1.00265091003727,-1.,1.66846059277303));
#21601=CARTESIAN_POINT('Ctrl Pts',(-1.00692206696414,-1.,1.67250335383293));
#21602=CARTESIAN_POINT('Ctrl Pts',(-1.01123236493511,-1.,1.67648246776464));
#21603=CARTESIAN_POINT('Ctrl Pts',(-1.01561026162773,-1.,1.68044289894798));
#21604=CARTESIAN_POINT('Ctrl Pts',(-1.02006795074201,-1.,1.68440578021706));
#21605=CARTESIAN_POINT('Ctrl Pts',(-1.02460180535255,-1.,1.68836910178447));
#21606=CARTESIAN_POINT('Ctrl Pts',(-1.02919977579147,-1.,1.69231840863458));
#21607=CARTESIAN_POINT('Ctrl Pts',(-1.03384646003588,-1.,1.69623414782771));
#21608=CARTESIAN_POINT('Ctrl Pts',(-1.03852922490789,-1.,1.70010052930962));
#21609=CARTESIAN_POINT('Ctrl Pts',(-1.04324363334554,-1.,1.70391338707982));
#21610=CARTESIAN_POINT('Ctrl Pts',(-1.04799085404995,-1.,1.70767646263649));
#21611=CARTESIAN_POINT('Ctrl Pts',(-1.05277517202855,-1.,1.71139783543989));
#21612=CARTESIAN_POINT('Ctrl Pts',(-1.05760163192479,-1.,1.7150865442702));
#21613=CARTESIAN_POINT('Ctrl Pts',(-1.06247324680647,-1.,1.71874858456904));
#21614=CARTESIAN_POINT('Ctrl Pts',(-1.06738966975462,-1.,1.72238500928453));
#21615=CARTESIAN_POINT('Ctrl Pts',(-1.07234866990252,-1.,1.72599406198488));
#21616=CARTESIAN_POINT('Ctrl Pts',(-1.0773470373727,-1.,1.72957248977424));
#21617=CARTESIAN_POINT('Ctrl Pts',(-1.08238162784749,-1.,1.73311705663407));
#21618=CARTESIAN_POINT('Ctrl Pts',(-1.08745056285427,-1.,1.73662628326091));
#21619=CARTESIAN_POINT('Ctrl Pts',(-1.09255329056493,-1.,1.74010053962247));
#21620=CARTESIAN_POINT('Ctrl Pts',(-1.09768999241225,-1.,1.74354119236208));
#21621=CARTESIAN_POINT('Ctrl Pts',(-1.10286118991143,-1.,1.74695004214923));
#21622=CARTESIAN_POINT('Ctrl Pts',(-1.10806728183007,-1.,1.7503286607592));
#21623=CARTESIAN_POINT('Ctrl Pts',(-1.11330807582551,-1.,1.7536777209463));
#21624=CARTESIAN_POINT('Ctrl Pts',(-1.11858293216763,-1.,1.75699720772105));
#21625=CARTESIAN_POINT('Ctrl Pts',(-1.12389096855086,-1.,1.76028671825096));
#21626=CARTESIAN_POINT('Ctrl Pts',(-1.12923123555075,-1.,1.7635457196617));
#21627=CARTESIAN_POINT('Ctrl Pts',(-1.1346029180462,-1.,1.76677384551862));
#21628=CARTESIAN_POINT('Ctrl Pts',(-1.14000548336975,-1.,1.76997111386769));
#21629=CARTESIAN_POINT('Ctrl Pts',(-1.1454385822692,-1.,1.77313777896194));
#21630=CARTESIAN_POINT('Ctrl Pts',(-1.15090197841515,-1.,1.7762742255701));
#21631=CARTESIAN_POINT('Ctrl Pts',(-1.15639547194698,-1.,1.77938085564275));
#21632=CARTESIAN_POINT('Ctrl Pts',(-1.16191881298499,-1.,1.78245795881009));
#21633=CARTESIAN_POINT('Ctrl Pts',(-1.16747166312303,-1.,1.78550566040443));
#21634=CARTESIAN_POINT('Ctrl Pts',(-1.17305363177328,-1.,1.78852398877616));
#21635=CARTESIAN_POINT('Ctrl Pts',(-1.17866429440809,-1.,1.79151291552689));
#21636=CARTESIAN_POINT('Ctrl Pts',(-1.18430321697432,-1.,1.79447240321515));
#21637=CARTESIAN_POINT('Ctrl Pts',(-1.18996997934445,-1.,1.79740245923478));
#21638=CARTESIAN_POINT('Ctrl Pts',(-1.19566418930242,-1.,1.80030314369879));
#21639=CARTESIAN_POINT('Ctrl Pts',(-1.20138548938974,-1.,1.80317454838603));
#21640=CARTESIAN_POINT('Ctrl Pts',(-1.20713356605475,-1.,1.80601678480707));
#21641=CARTESIAN_POINT('Ctrl Pts',(-1.21290815708314,-1.,1.80882996917129));
#21642=CARTESIAN_POINT('Ctrl Pts',(-1.21870906103557,-1.,1.81161420806656));
#21643=CARTESIAN_POINT('Ctrl Pts',(-1.2245361330495,-1.,1.81436959210434));
#21644=CARTESIAN_POINT('Ctrl Pts',(-1.2292186489137,-1.,1.8165508718364));
#21645=CARTESIAN_POINT('Ctrl Pts',(-1.2327422452705,-1.,1.81817389921279));
#21646=CARTESIAN_POINT('Ctrl Pts',(-1.23509651170476,-1.,1.81925017193666));
#21647=CARTESIAN_POINT('Ctrl Pts',(-1.23627494547115,-1.,1.81978687191668));
#21648=CARTESIAN_POINT('',(-1.34869019493419,-1.,1.73811241238545));
#21649=CARTESIAN_POINT('',(-1.23627494547115,-1.,1.81978687191668));
#21650=CARTESIAN_POINT('',(-1.15624053661742,-1.,1.31362392696032));
#21651=CARTESIAN_POINT('Ctrl Pts',(-1.34869019493419,-1.,1.73811241238545));
#21652=CARTESIAN_POINT('Ctrl Pts',(-1.34854391898045,-1.,1.73682580585691));
#21653=CARTESIAN_POINT('Ctrl Pts',(-1.34824783112887,-1.,1.73425417885907));
#21654=CARTESIAN_POINT('Ctrl Pts',(-1.34779309152035,-1.,1.7304014965394));
#21655=CARTESIAN_POINT('Ctrl Pts',(-1.34716554819527,-1.,1.72527410680674));
#21656=CARTESIAN_POINT('Ctrl Pts',(-1.34634568653227,-1.,1.7188807715049));
#21657=CARTESIAN_POINT('Ctrl Pts',(-1.34549029589416,-1.,1.71250340686822));
#21658=CARTESIAN_POINT('Ctrl Pts',(-1.34459924533831,-1.,1.70614212266738));
#21659=CARTESIAN_POINT('Ctrl Pts',(-1.34367237124483,-1.,1.69979707754427));
#21660=CARTESIAN_POINT('Ctrl Pts',(-1.34270948206319,-1.,1.6934684849687));
#21661=CARTESIAN_POINT('Ctrl Pts',(-1.341710374848,-1.,1.68715660868764));
#21662=CARTESIAN_POINT('Ctrl Pts',(-1.34067485185203,-1.,1.68086176030362));
#21663=CARTESIAN_POINT('Ctrl Pts',(-1.3396027347034,-1.,1.67458429426086));
#21664=CARTESIAN_POINT('Ctrl Pts',(-1.33849388654388,-1.,1.66832460783989));
#21665=CARTESIAN_POINT('Ctrl Pts',(-1.33734820885262,-1.,1.66208312541983));
#21666=CARTESIAN_POINT('Ctrl Pts',(-1.33616559745172,-1.,1.65586025952593));
#21667=CARTESIAN_POINT('Ctrl Pts',(-1.33494590467993,-1.,1.6496563728683));
#21668=CARTESIAN_POINT('Ctrl Pts',(-1.33368890676572,-1.,1.6434717485603));
#21669=CARTESIAN_POINT('Ctrl Pts',(-1.33239425103724,-1.,1.63730653475089));
#21670=CARTESIAN_POINT('Ctrl Pts',(-1.33106149345645,-1.,1.63116079730923));
#21671=CARTESIAN_POINT('Ctrl Pts',(-1.3296901950568,-1.,1.62503464209797));
#21672=CARTESIAN_POINT('Ctrl Pts',(-1.32828000610449,-1.,1.61892832270724));
#21673=CARTESIAN_POINT('Ctrl Pts',(-1.32683074483356,-1.,1.6128423401575));
#21674=CARTESIAN_POINT('Ctrl Pts',(-1.32534250785782,-1.,1.60677758290954));
#21675=CARTESIAN_POINT('Ctrl Pts',(-1.32381550858256,-1.,1.60073511858687));
#21676=CARTESIAN_POINT('Ctrl Pts',(-1.32224985747682,-1.,1.59471591079403));
#21677=CARTESIAN_POINT('Ctrl Pts',(-1.32064537110892,-1.,1.58872057258245));
#21678=CARTESIAN_POINT('Ctrl Pts',(-1.31900135021432,-1.,1.58274907898834));
#21679=CARTESIAN_POINT('Ctrl Pts',(-1.31731642317187,-1.,1.5768005650559));
#21680=CARTESIAN_POINT('Ctrl Pts',(-1.31558903860016,-1.,1.57087397835723));
#21681=CARTESIAN_POINT('Ctrl Pts',(-1.31381795281002,-1.,1.56496872402353));
#21682=CARTESIAN_POINT('Ctrl Pts',(-1.31200264341696,-1.,1.55908521254821));
#21683=CARTESIAN_POINT('Ctrl Pts',(-1.31014393684222,-1.,1.55322568759481));
#21684=CARTESIAN_POINT('Ctrl Pts',(-1.30824393907473,-1.,1.54739413957185));
#21685=CARTESIAN_POINT('Ctrl Pts',(-1.30630475189556,-1.,1.54159462645432));
#21686=CARTESIAN_POINT('Ctrl Pts',(-1.30432735639489,-1.,1.53582981268977));
#21687=CARTESIAN_POINT('Ctrl Pts',(-1.30231064395568,-1.,1.53009970283891));
#21688=CARTESIAN_POINT('Ctrl Pts',(-1.30024984366328,-1.,1.52439957861062));
#21689=CARTESIAN_POINT('Ctrl Pts',(-1.29813791800747,-1.,1.51872184912724));
#21690=CARTESIAN_POINT('Ctrl Pts',(-1.29596850710509,-1.,1.51305994241402));
#21691=CARTESIAN_POINT('Ctrl Pts',(-1.29373841372842,-1.,1.50741159078365));
#21692=CARTESIAN_POINT('Ctrl Pts',(-1.29145022885181,-1.,1.50178230149776));
#21693=CARTESIAN_POINT('Ctrl Pts',(-1.28911506584254,-1.,1.49618896881754));
#21694=CARTESIAN_POINT('Ctrl Pts',(-1.2867467611644,-1.,1.4906522831278));
#21695=CARTESIAN_POINT('Ctrl Pts',(-1.28435533880201,-1.,1.4851881711891));
#21696=CARTESIAN_POINT('Ctrl Pts',(-1.28194158939517,-1.,1.47980070347095));
#21697=CARTESIAN_POINT('Ctrl Pts',(-1.2794891824849,-1.,1.4744717526707));
#21698=CARTESIAN_POINT('Ctrl Pts',(-1.27696414831089,-1.,1.46916035917133));
#21699=CARTESIAN_POINT('Ctrl Pts',(-1.27433119897822,-1.,1.46382431332476));
#21700=CARTESIAN_POINT('Ctrl Pts',(-1.27156805265289,-1.,1.45843906294697));
#21701=CARTESIAN_POINT('Ctrl Pts',(-1.2686778680489,-1.,1.45301422764247));
#21702=CARTESIAN_POINT('Ctrl Pts',(-1.26570925118868,-1.,1.44761985001662));
#21703=CARTESIAN_POINT('Ctrl Pts',(-1.26273903323859,-1.,1.44236470511303));
#21704=CARTESIAN_POINT('Ctrl Pts',(-1.25983531012005,-1.,1.43734919180848));
#21705=CARTESIAN_POINT('Ctrl Pts',(-1.25702687965755,-1.,1.43262645609691));
#21706=CARTESIAN_POINT('Ctrl Pts',(-1.25426945222639,-1.,1.42815938799387));
#21707=CARTESIAN_POINT('Ctrl Pts',(-1.2514145557001,-1.,1.42378102115575));
#21708=CARTESIAN_POINT('Ctrl Pts',(-1.24824430986571,-1.,1.41923722596025));
#21709=CARTESIAN_POINT('Ctrl Pts',(-1.24450600513056,-1.,1.41422913175179));
#21710=CARTESIAN_POINT('Ctrl Pts',(-1.23994455029534,-1.,1.40845295531283));
#21711=CARTESIAN_POINT('Ctrl Pts',(-1.23434087290423,-1.,1.40164708206106));
#21712=CARTESIAN_POINT('Ctrl Pts',(-1.22752961899387,-1.,1.39361389568796));
#21713=CARTESIAN_POINT('Ctrl Pts',(-1.21938737280852,-1.,1.38420564527715));
#21714=CARTESIAN_POINT('Ctrl Pts',(-1.20982812925645,-1.,1.37331915607905));
#21715=CARTESIAN_POINT('Ctrl Pts',(-1.1987959077932,-1.,1.36088705043885));
#21716=CARTESIAN_POINT('Ctrl Pts',(-1.18625865667441,-1.,1.34687054001093));
#21717=CARTESIAN_POINT('Ctrl Pts',(-1.17501305789857,-1.,1.33437539347008));
#21718=CARTESIAN_POINT('Ctrl Pts',(-1.16589330093588,-1.,1.32428080721772));
#21719=CARTESIAN_POINT('Ctrl Pts',(-1.15950888730809,-1.,1.31722977216397));
#21720=CARTESIAN_POINT('Ctrl Pts',(-1.15624053661742,-1.,1.31362392696032));
#21721=CARTESIAN_POINT('',(-1.31362392696033,-1.,1.15624053661742));
#21722=CARTESIAN_POINT('Origin',(0.,-1.,0.));
#21723=CARTESIAN_POINT('',(-1.73811241238545,-1.,1.34869019493419));
#21724=CARTESIAN_POINT('Ctrl Pts',(-1.31362392696033,-1.,1.15624053661742));
#21725=CARTESIAN_POINT('Ctrl Pts',(-1.3172297721596,-1.,1.15950888730433));
#21726=CARTESIAN_POINT('Ctrl Pts',(-1.32428080720544,-1.,1.16589330092532));
#21727=CARTESIAN_POINT('Ctrl Pts',(-1.33437539344842,-1.,1.17501305787994));
#21728=CARTESIAN_POINT('Ctrl Pts',(-1.34687053998157,-1.,1.18625865664915));
#21729=CARTESIAN_POINT('Ctrl Pts',(-1.36088705040677,-1.,1.1987959077656));
#21730=CARTESIAN_POINT('Ctrl Pts',(-1.37331915604962,-1.,1.20982812923113));
#21731=CARTESIAN_POINT('Ctrl Pts',(-1.38420564525391,-1.,1.21938737278853));
#21732=CARTESIAN_POINT('Ctrl Pts',(-1.39361389567257,-1.,1.22752961898063));
#21733=CARTESIAN_POINT('Ctrl Pts',(-1.40164708205345,-1.,1.23434087289768));
#21734=CARTESIAN_POINT('Ctrl Pts',(-1.40845295531151,-1.,1.23994455029421));
#21735=CARTESIAN_POINT('Ctrl Pts',(-1.41422913175437,-1.,1.24450600513278));
#21736=CARTESIAN_POINT('Ctrl Pts',(-1.41923722596421,-1.,1.24824430986911));
#21737=CARTESIAN_POINT('Ctrl Pts',(-1.42378102115911,-1.,1.25141455570299));
#21738=CARTESIAN_POINT('Ctrl Pts',(-1.42815938799555,-1.,1.25426945222783));
#21739=CARTESIAN_POINT('Ctrl Pts',(-1.43262645609679,-1.,1.25702687965744));
#21740=CARTESIAN_POINT('Ctrl Pts',(-1.43734919180719,-1.,1.25983531011894));
#21741=CARTESIAN_POINT('Ctrl Pts',(-1.44236470511145,-1.,1.26273903323723));
#21742=CARTESIAN_POINT('Ctrl Pts',(-1.44761985001544,-1.,1.26570925118767));
#21743=CARTESIAN_POINT('Ctrl Pts',(-1.45301422764205,-1.,1.26867786804854));
#21744=CARTESIAN_POINT('Ctrl Pts',(-1.45843906294725,-1.,1.27156805265312));
#21745=CARTESIAN_POINT('Ctrl Pts',(-1.4638243133254,-1.,1.27433119897877));
#21746=CARTESIAN_POINT('Ctrl Pts',(-1.46916035917197,-1.,1.27696414831144));
#21747=CARTESIAN_POINT('Ctrl Pts',(-1.4744717526711,-1.,1.27948918248524));
#21748=CARTESIAN_POINT('Ctrl Pts',(-1.47980070347102,-1.,1.28194158939522));
#21749=CARTESIAN_POINT('Ctrl Pts',(-1.48518817118891,-1.,1.28435533880184));
#21750=CARTESIAN_POINT('Ctrl Pts',(-1.4906522831275,-1.,1.28674676116415));
#21751=CARTESIAN_POINT('Ctrl Pts',(-1.49618896881729,-1.,1.28911506584232));
#21752=CARTESIAN_POINT('Ctrl Pts',(-1.50178230149764,-1.,1.29145022885171));
#21753=CARTESIAN_POINT('Ctrl Pts',(-1.50741159078367,-1.,1.29373841372843));
#21754=CARTESIAN_POINT('Ctrl Pts',(-1.51305994241412,-1.,1.29596850710518));
#21755=CARTESIAN_POINT('Ctrl Pts',(-1.51872184912735,-1.,1.29813791800757));
#21756=CARTESIAN_POINT('Ctrl Pts',(-1.5243995786107,-1.,1.30024984366334));
#21757=CARTESIAN_POINT('Ctrl Pts',(-1.53009970283893,-1.,1.3023106439557));
#21758=CARTESIAN_POINT('Ctrl Pts',(-1.53582981268976,-1.,1.30432735639487));
#21759=CARTESIAN_POINT('Ctrl Pts',(-1.54159462645428,-1.,1.30630475189553));
#21760=CARTESIAN_POINT('Ctrl Pts',(-1.54739413957183,-1.,1.30824393907471));
#21761=CARTESIAN_POINT('Ctrl Pts',(-1.55322568759481,-1.,1.31014393684221));
#21762=CARTESIAN_POINT('Ctrl Pts',(-1.55908521254822,-1.,1.31200264341696));
#21763=CARTESIAN_POINT('Ctrl Pts',(-1.56496872402352,-1.,1.31381795281002));
#21764=CARTESIAN_POINT('Ctrl Pts',(-1.57087397835721,-1.,1.31558903860015));
#21765=CARTESIAN_POINT('Ctrl Pts',(-1.57680056505585,-1.,1.31731642317183));
#21766=CARTESIAN_POINT('Ctrl Pts',(-1.58274907898829,-1.,1.31900135021428));
#21767=CARTESIAN_POINT('Ctrl Pts',(-1.58872057258244,-1.,1.32064537110891));
#21768=CARTESIAN_POINT('Ctrl Pts',(-1.59471591079408,-1.,1.32224985747686));
#21769=CARTESIAN_POINT('Ctrl Pts',(-1.600735118587,-1.,1.32381550858266));
#21770=CARTESIAN_POINT('Ctrl Pts',(-1.6067775829097,-1.,1.32534250785794));
#21771=CARTESIAN_POINT('Ctrl Pts',(-1.61284234015762,-1.,1.32683074483365));
#21772=CARTESIAN_POINT('Ctrl Pts',(-1.61892832270723,-1.,1.32828000610448));
#21773=CARTESIAN_POINT('Ctrl Pts',(-1.62503464209777,-1.,1.32969019505665));
#21774=CARTESIAN_POINT('Ctrl Pts',(-1.63116079730887,-1.,1.33106149345618));
#21775=CARTESIAN_POINT('Ctrl Pts',(-1.6373065347505,-1.,1.33239425103694));
#21776=CARTESIAN_POINT('Ctrl Pts',(-1.64347174856007,-1.,1.33368890676554));
#21777=CARTESIAN_POINT('Ctrl Pts',(-1.64965637286843,-1.,1.33494590468003));
#21778=CARTESIAN_POINT('Ctrl Pts',(-1.65586025952651,-1.,1.33616559745217));
#21779=CARTESIAN_POINT('Ctrl Pts',(-1.66208312542073,-1.,1.33734820885331));
#21780=CARTESIAN_POINT('Ctrl Pts',(-1.66832460784078,-1.,1.33849388654458));
#21781=CARTESIAN_POINT('Ctrl Pts',(-1.67458429426126,-1.,1.33960273470372));
#21782=CARTESIAN_POINT('Ctrl Pts',(-1.68086176030308,-1.,1.3406748518516));
#21783=CARTESIAN_POINT('Ctrl Pts',(-1.68715660868602,-1.,1.34171037484673));
#21784=CARTESIAN_POINT('Ctrl Pts',(-1.6934684849664,-1.,1.34270948206139));
#21785=CARTESIAN_POINT('Ctrl Pts',(-1.69979707754221,-1.,1.34367237124322));
#21786=CARTESIAN_POINT('Ctrl Pts',(-1.70614212266676,-1.,1.34459924533783));
#21787=CARTESIAN_POINT('Ctrl Pts',(-1.71250340687011,-1.,1.34549029589563));
#21788=CARTESIAN_POINT('Ctrl Pts',(-1.7188807715095,-1.,1.34634568653586));
#21789=CARTESIAN_POINT('Ctrl Pts',(-1.72527410681298,-1.,1.34716554820013));
#21790=CARTESIAN_POINT('Ctrl Pts',(-1.73040149654497,-1.,1.3477930915247));
#21791=CARTESIAN_POINT('Ctrl Pts',(-1.73425417886255,-1.,1.34824783113158));
#21792=CARTESIAN_POINT('Ctrl Pts',(-1.73682580585819,-1.,1.34854391898145));
#21793=CARTESIAN_POINT('Ctrl Pts',(-1.73811241238545,-1.,1.34869019493419));
#21794=CARTESIAN_POINT('',(-1.81978687191668,-1.,1.23627494547115));
#21795=CARTESIAN_POINT('',(-1.73811241238545,-1.,1.34869019493419));
#21796=CARTESIAN_POINT('',(-1.5055822144029,-1.,0.892032620296855));
#21797=CARTESIAN_POINT('Ctrl Pts',(-1.81978687191668,-1.,1.23627494547115));
#21798=CARTESIAN_POINT('Ctrl Pts',(-1.81925017193531,-1.,1.23509651170384));
#21799=CARTESIAN_POINT('Ctrl Pts',(-1.81817389920914,-1.,1.23274224526804));
#21800=CARTESIAN_POINT('Ctrl Pts',(-1.81655087183054,-1.,1.22921864890975));
#21801=CARTESIAN_POINT('Ctrl Pts',(-1.81436959209778,-1.,1.22453613304507));
#21802=CARTESIAN_POINT('Ctrl Pts',(-1.81161420806172,-1.,1.2187090610323));
#21803=CARTESIAN_POINT('Ctrl Pts',(-1.80882996916931,-1.,1.2129081570818));
#21804=CARTESIAN_POINT('Ctrl Pts',(-1.80601678480772,-1.,1.20713356605519));
#21805=CARTESIAN_POINT('Ctrl Pts',(-1.8031745483882,-1.,1.2013854893912));
#21806=CARTESIAN_POINT('Ctrl Pts',(-1.80030314370121,-1.,1.19566418930405));
#21807=CARTESIAN_POINT('Ctrl Pts',(-1.79740245923649,-1.,1.1899699793456));
#21808=CARTESIAN_POINT('Ctrl Pts',(-1.79447240321572,-1.,1.18430321697471));
#21809=CARTESIAN_POINT('Ctrl Pts',(-1.79151291552646,-1.,1.17866429440781));
#21810=CARTESIAN_POINT('Ctrl Pts',(-1.78852398877523,-1.,1.17305363177265));
#21811=CARTESIAN_POINT('Ctrl Pts',(-1.78550566040349,-1.,1.16747166312239));
#21812=CARTESIAN_POINT('Ctrl Pts',(-1.78245795880949,-1.,1.16191881298458));
#21813=CARTESIAN_POINT('Ctrl Pts',(-1.77938085564261,-1.,1.15639547194689));
#21814=CARTESIAN_POINT('Ctrl Pts',(-1.77627422557034,-1.,1.15090197841531));
#21815=CARTESIAN_POINT('Ctrl Pts',(-1.77313777896234,-1.,1.14543858226948));
#21816=CARTESIAN_POINT('Ctrl Pts',(-1.76997111386806,-1.,1.14000548337));
#21817=CARTESIAN_POINT('Ctrl Pts',(-1.76677384551883,-1.,1.13460291804635));
#21818=CARTESIAN_POINT('Ctrl Pts',(-1.76354571966171,-1.,1.12923123555076));
#21819=CARTESIAN_POINT('Ctrl Pts',(-1.76028671825084,-1.,1.12389096855078));
#21820=CARTESIAN_POINT('Ctrl Pts',(-1.75699720772089,-1.,1.11858293216752));
#21821=CARTESIAN_POINT('Ctrl Pts',(-1.75367772094617,-1.,1.11330807582542));
#21822=CARTESIAN_POINT('Ctrl Pts',(-1.75032866075914,-1.,1.10806728183003));
#21823=CARTESIAN_POINT('Ctrl Pts',(-1.74695004214924,-1.,1.10286118991144));
#21824=CARTESIAN_POINT('Ctrl Pts',(-1.74354119236212,-1.,1.09768999241229));
#21825=CARTESIAN_POINT('Ctrl Pts',(-1.74010053962252,-1.,1.09255329056496));
#21826=CARTESIAN_POINT('Ctrl Pts',(-1.73662628326093,-1.,1.08745056285429));
#21827=CARTESIAN_POINT('Ctrl Pts',(-1.73311705663407,-1.,1.08238162784749));
#21828=CARTESIAN_POINT('Ctrl Pts',(-1.72957248977424,-1.,1.0773470373727));
#21829=CARTESIAN_POINT('Ctrl Pts',(-1.72599406198489,-1.,1.07234866990252));
#21830=CARTESIAN_POINT('Ctrl Pts',(-1.72238500928456,-1.,1.06738966975463));
#21831=CARTESIAN_POINT('Ctrl Pts',(-1.71874858456908,-1.,1.0624732468065));
#21832=CARTESIAN_POINT('Ctrl Pts',(-1.71508654427022,-1.,1.05760163192481));
#21833=CARTESIAN_POINT('Ctrl Pts',(-1.71139783543986,-1.,1.05277517202854));
#21834=CARTESIAN_POINT('Ctrl Pts',(-1.70767646263641,-1.,1.0479908540499));
#21835=CARTESIAN_POINT('Ctrl Pts',(-1.70391338707969,-1.,1.04324363334546));
#21836=CARTESIAN_POINT('Ctrl Pts',(-1.70010052930951,-1.,1.03852922490782));
#21837=CARTESIAN_POINT('Ctrl Pts',(-1.69623414782769,-1.,1.03384646003587));
#21838=CARTESIAN_POINT('Ctrl Pts',(-1.69231840863471,-1.,1.02919977579155));
#21839=CARTESIAN_POINT('Ctrl Pts',(-1.68836910178475,-1.,1.02460180535272));
#21840=CARTESIAN_POINT('Ctrl Pts',(-1.68440578021739,-1.,1.02006795074222));
#21841=CARTESIAN_POINT('Ctrl Pts',(-1.6804428989482,-1.,1.01561026162787));
#21842=CARTESIAN_POINT('Ctrl Pts',(-1.67648246776457,-1.,1.01123236493507));
#21843=CARTESIAN_POINT('Ctrl Pts',(-1.67250335383248,-1.,1.00692206696387));
#21844=CARTESIAN_POINT('Ctrl Pts',(-1.66846059277231,-1.,1.00265091003682));
#21845=CARTESIAN_POINT('Ctrl Pts',(-1.66430758030304,-1.,0.998389654952317));
#21846=CARTESIAN_POINT('Ctrl Pts',(-1.66001553809916,-1.,0.994121836661116));
#21847=CARTESIAN_POINT('Ctrl Pts',(-1.65559044289746,-1.,0.98985562785445));
#21848=CARTESIAN_POINT('Ctrl Pts',(-1.6511001661277,-1.,0.985642622921626));
#21849=CARTESIAN_POINT('Ctrl Pts',(-1.64665139190834,-1.,0.981562530940574));
#21850=CARTESIAN_POINT('Ctrl Pts',(-1.64233990826831,-1.,0.977689794120297));
#21851=CARTESIAN_POINT('Ctrl Pts',(-1.63820952658157,-1.,0.974066058287501));
#21852=CARTESIAN_POINT('Ctrl Pts',(-1.63420665729609,-1.,0.970669715996356));
#21853=CARTESIAN_POINT('Ctrl Pts',(-1.63013849959083,-1.,0.967387853228041));
#21854=CARTESIAN_POINT('Ctrl Pts',(-1.6257193066974,-1.,0.964046107037821));
#21855=CARTESIAN_POINT('Ctrl Pts',(-1.62061638139929,-1.,0.960438326099958));
#21856=CARTESIAN_POINT('Ctrl Pts',(-1.61449324337233,-1.,0.956354422921573));
#21857=CARTESIAN_POINT('Ctrl Pts',(-1.60706069897794,-1.,0.951613284361248));
#21858=CARTESIAN_POINT('Ctrl Pts',(-1.59810042045408,-1.,0.946078063325796));
#21859=CARTESIAN_POINT('Ctrl Pts',(-1.58744937489796,-1.,0.939646377909319));
#21860=CARTESIAN_POINT('Ctrl Pts',(-1.57499388385561,-1.,0.932246680128849));
#21861=CARTESIAN_POINT('Ctrl Pts',(-1.56065988582509,-1.,0.923832188966322));
#21862=CARTESIAN_POINT('Ctrl Pts',(-1.54440491152808,-1.,0.91437591904658));
#21863=CARTESIAN_POINT('Ctrl Pts',(-1.52984849890434,-1.,0.905967409640499));
#21864=CARTESIAN_POINT('Ctrl Pts',(-1.51805569591479,-1.,0.89918504749193));
#21865=CARTESIAN_POINT('Ctrl Pts',(-1.50980486807181,-1.,0.894452006967538));
#21866=CARTESIAN_POINT('Ctrl Pts',(-1.5055822144029,-1.,0.892032620296855));
#21867=CARTESIAN_POINT('',(-1.60662857109684,-1.,0.693717979106305));
#21868=CARTESIAN_POINT('Origin',(0.,-1.,0.));
#21869=CARTESIAN_POINT('',(-2.0698113262342,-1.,0.7455743247944));
#21870=CARTESIAN_POINT('Ctrl Pts',(-1.60662857109684,-1.,0.693717979106305));
#21871=CARTESIAN_POINT('Ctrl Pts',(-1.61106790957619,-1.,0.69571209787897));
#21872=CARTESIAN_POINT('Ctrl Pts',(-1.61974673471117,-1.,0.699605146398837));
#21873=CARTESIAN_POINT('Ctrl Pts',(-1.6321654166204,-1.,0.705159151977294));
#21874=CARTESIAN_POINT('Ctrl Pts',(-1.64752408828442,-1.,0.711993139340447));
#21875=CARTESIAN_POINT('Ctrl Pts',(-1.66472880551777,-1.,0.71958543378795));
#21876=CARTESIAN_POINT('Ctrl Pts',(-1.67996158451922,-1.,0.726235967982445));
#21877=CARTESIAN_POINT('Ctrl Pts',(-1.69326921972915,-1.,0.731963238685357));
#21878=CARTESIAN_POINT('Ctrl Pts',(-1.70473309004249,-1.,0.736799665716932));
#21879=CARTESIAN_POINT('Ctrl Pts',(-1.71447789751001,-1.,0.74079516202821));
#21880=CARTESIAN_POINT('Ctrl Pts',(-1.72268229916769,-1.,0.744021445433093));
#21881=CARTESIAN_POINT('Ctrl Pts',(-1.72958533647714,-1.,0.746574710097752));
#21882=CARTESIAN_POINT('Ctrl Pts',(-1.7355035168033,-1.,0.74858246295687));
#21883=CARTESIAN_POINT('Ctrl Pts',(-1.74080458267114,-1.,0.750193435981249));
#21884=CARTESIAN_POINT('Ctrl Pts',(-1.74585086852502,-1.,0.751555614164482));
#21885=CARTESIAN_POINT('Ctrl Pts',(-1.75095139468794,-1.,0.752797683531314));
#21886=CARTESIAN_POINT('Ctrl Pts',(-1.75631083600019,-1.,0.754009254027829));
#21887=CARTESIAN_POINT('Ctrl Pts',(-1.76197817240128,-1.,0.755220979974461));
#21888=CARTESIAN_POINT('Ctrl Pts',(-1.76789396002998,-1.,0.75642189602781));
#21889=CARTESIAN_POINT('Ctrl Pts',(-1.77394167108292,-1.,0.757578264077029));
#21890=CARTESIAN_POINT('Ctrl Pts',(-1.77999411220945,-1.,0.758650626677518));
#21891=CARTESIAN_POINT('Ctrl Pts',(-1.78596964884604,-1.,0.759614401110189));
#21892=CARTESIAN_POINT('Ctrl Pts',(-1.7918581561088,-1.,0.760469555880749));
#21893=CARTESIAN_POINT('Ctrl Pts',(-1.79768986997783,-1.,0.761229695230558));
#21894=CARTESIAN_POINT('Ctrl Pts',(-1.80351583877342,-1.,0.761915336443547));
#21895=CARTESIAN_POINT('Ctrl Pts',(-1.80938551463965,-1.,0.762546129463938));
#21896=CARTESIAN_POINT('Ctrl Pts',(-1.8153211840553,-1.,0.763132003836634));
#21897=CARTESIAN_POINT('Ctrl Pts',(-1.82131873145266,-1.,0.763673465462726));
#21898=CARTESIAN_POINT('Ctrl Pts',(-1.82735991200065,-1.,0.764165902605995));
#21899=CARTESIAN_POINT('Ctrl Pts',(-1.83342077227142,-1.,0.764602549687853));
#21900=CARTESIAN_POINT('Ctrl Pts',(-1.83948181064835,-1.,0.764978057881737));
#21901=CARTESIAN_POINT('Ctrl Pts',(-1.84553698875924,-1.,0.765291664862029));
#21902=CARTESIAN_POINT('Ctrl Pts',(-1.85158945130063,-1.,0.765545710619062));
#21903=CARTESIAN_POINT('Ctrl Pts',(-1.85764741390394,-1.,0.765744212909318));
#21904=CARTESIAN_POINT('Ctrl Pts',(-1.86372027063312,-1.,0.765891519092547));
#21905=CARTESIAN_POINT('Ctrl Pts',(-1.86981398314341,-1.,0.765990708546091));
#21906=CARTESIAN_POINT('Ctrl Pts',(-1.87592888967883,-1.,0.766042837036744));
#21907=CARTESIAN_POINT('Ctrl Pts',(-1.88206215302561,-1.,0.766047794851864));
#21908=CARTESIAN_POINT('Ctrl Pts',(-1.88820926433409,-1.,0.766004837062091));
#21909=CARTESIAN_POINT('Ctrl Pts',(-1.89436577771388,-1.,0.765913193856978));
#21910=CARTESIAN_POINT('Ctrl Pts',(-1.90052930393596,-1.,0.765772772593386));
#21911=CARTESIAN_POINT('Ctrl Pts',(-1.90669961402356,-1.,0.765584196937919));
#21912=CARTESIAN_POINT('Ctrl Pts',(-1.91287765805169,-1.,0.765348465884722));
#21913=CARTESIAN_POINT('Ctrl Pts',(-1.91906491634196,-1.,0.765066729667088));
#21914=CARTESIAN_POINT('Ctrl Pts',(-1.92526263537048,-1.,0.764740025488211));
#21915=CARTESIAN_POINT('Ctrl Pts',(-1.93147105496382,-1.,0.76436901067394));
#21916=CARTESIAN_POINT('Ctrl Pts',(-1.93768964875886,-1.,0.763954049121458));
#21917=CARTESIAN_POINT('Ctrl Pts',(-1.9439174661764,-1.,0.763495333538629));
#21918=CARTESIAN_POINT('Ctrl Pts',(-1.95015342590024,-1.,0.762992990878769));
#21919=CARTESIAN_POINT('Ctrl Pts',(-1.95639665309869,-1.,0.762447203806179));
#21920=CARTESIAN_POINT('Ctrl Pts',(-1.96264672744186,-1.,0.761858300014423));
#21921=CARTESIAN_POINT('Ctrl Pts',(-1.96890351582499,-1.,0.76122669048382));
#21922=CARTESIAN_POINT('Ctrl Pts',(-1.97516705321494,-1.,0.760552825409757));
#21923=CARTESIAN_POINT('Ctrl Pts',(-1.98143741418172,-1.,0.75983714745219));
#21924=CARTESIAN_POINT('Ctrl Pts',(-1.98771456680874,-1.,0.759080037802488));
#21925=CARTESIAN_POINT('Ctrl Pts',(-1.99399831098817,-1.,0.758281796766761));
#21926=CARTESIAN_POINT('Ctrl Pts',(-2.00028834739178,-1.,0.757442676862724));
#21927=CARTESIAN_POINT('Ctrl Pts',(-2.0065843158773,-1.,0.75656290464667));
#21928=CARTESIAN_POINT('Ctrl Pts',(-2.01288584328084,-1.,0.755642704957865));
#21929=CARTESIAN_POINT('Ctrl Pts',(-2.01919259405809,-1.,0.754682330722816));
#21930=CARTESIAN_POINT('Ctrl Pts',(-2.02550428623313,-1.,0.753682061112768));
#21931=CARTESIAN_POINT('Ctrl Pts',(-2.03182068456221,-1.,0.752642180487211));
#21932=CARTESIAN_POINT('Ctrl Pts',(-2.03814160092099,-1.,0.751562963361115));
#21933=CARTESIAN_POINT('Ctrl Pts',(-2.04446689147979,-1.,0.750444657875576));
#21934=CARTESIAN_POINT('Ctrl Pts',(-2.05079645592154,-1.,0.749287468665046));
#21935=CARTESIAN_POINT('Ctrl Pts',(-2.05713023031006,-1.,0.748091554183802));
#21936=CARTESIAN_POINT('Ctrl Pts',(-2.06220058927826,-1.,0.747103932787919));
#21937=CARTESIAN_POINT('Ctrl Pts',(-2.06600523016815,-1.,0.7463458715442));
#21938=CARTESIAN_POINT('Ctrl Pts',(-2.06854248895728,-1.,0.745832791378367));
#21939=CARTESIAN_POINT('Ctrl Pts',(-2.0698113262342,-1.,0.7455743247944));
#21940=CARTESIAN_POINT('',(-2.11275013067528,-1.,0.61342227326009));
#21941=CARTESIAN_POINT('',(-2.0698113262342,-1.,0.7455743247944));
#21942=CARTESIAN_POINT('',(-1.7075470150345,-1.,0.383122945602004));
#21943=CARTESIAN_POINT('Ctrl Pts',(-2.11275013067528,-1.,0.61342227326009));
#21944=CARTESIAN_POINT('Ctrl Pts',(-2.11187554259986,-1.,0.6124673655618));
#21945=CARTESIAN_POINT('Ctrl Pts',(-2.11012443807238,-1.,0.610560911689899));
#21946=CARTESIAN_POINT('Ctrl Pts',(-2.1074919961518,-1.,0.607711315454876));
#21947=CARTESIAN_POINT('Ctrl Pts',(-2.10397049886949,-1.,0.60393203073603));
#21948=CARTESIAN_POINT('Ctrl Pts',(-2.0995493086477,-1.,0.599241616420533));
#21949=CARTESIAN_POINT('Ctrl Pts',(-2.0951087622027,-1.,0.594585006052162));
#21950=CARTESIAN_POINT('Ctrl Pts',(-2.09064881812129,-1.,0.589962365403406));
#21951=CARTESIAN_POINT('Ctrl Pts',(-2.08616943727951,-1.,0.585373918991617));
#21952=CARTESIAN_POINT('Ctrl Pts',(-2.08167059018418,-1.,0.580819952108063));
#21953=CARTESIAN_POINT('Ctrl Pts',(-2.07715226767559,-1.,0.576300797416844));
#21954=CARTESIAN_POINT('Ctrl Pts',(-2.07261449292824,-1.,0.571816823242603));
#21955=CARTESIAN_POINT('Ctrl Pts',(-2.06805732997334,-1.,0.567368421181087));
#21956=CARTESIAN_POINT('Ctrl Pts',(-2.06348090160589,-1.,0.562955993082261));
#21957=CARTESIAN_POINT('Ctrl Pts',(-2.05888537756462,-1.,0.558579940185151));
#21958=CARTESIAN_POINT('Ctrl Pts',(-2.05427091604413,-1.,0.554240657463906));
#21959=CARTESIAN_POINT('Ctrl Pts',(-2.04963761077958,-1.,0.549938525150295));
#21960=CARTESIAN_POINT('Ctrl Pts',(-2.04498544714588,-1.,0.54567390381743));
#21961=CARTESIAN_POINT('Ctrl Pts',(-2.04031422690527,-1.,0.541447120615659));
#21962=CARTESIAN_POINT('Ctrl Pts',(-2.03562362954037,-1.,0.537258489833262));
#21963=CARTESIAN_POINT('Ctrl Pts',(-2.03091336214426,-1.,0.533108355132976));
#21964=CARTESIAN_POINT('Ctrl Pts',(-2.0261832908329,-1.,0.528997127241914));
#21965=CARTESIAN_POINT('Ctrl Pts',(-2.02143356304698,-1.,0.524925318333476));
#21966=CARTESIAN_POINT('Ctrl Pts',(-2.01666477917286,-1.,0.52089359039937));
#21967=CARTESIAN_POINT('Ctrl Pts',(-2.01187773939242,-1.,0.516902681728687));
#21968=CARTESIAN_POINT('Ctrl Pts',(-2.00707309946949,-1.,0.512953306961792));
#21969=CARTESIAN_POINT('Ctrl Pts',(-2.00225107134734,-1.,0.509046069886157));
#21970=CARTESIAN_POINT('Ctrl Pts',(-1.99741107463572,-1.,0.505181361323026));
#21971=CARTESIAN_POINT('Ctrl Pts',(-1.99255149126155,-1.,0.501359287727146));
#21972=CARTESIAN_POINT('Ctrl Pts',(-1.98767044752932,-1.,0.497579909545574));
#21973=CARTESIAN_POINT('Ctrl Pts',(-1.98276658761821,-1.,0.493843476541494));
#21974=CARTESIAN_POINT('Ctrl Pts',(-1.97783973019229,-1.,0.490150627860952));
#21975=CARTESIAN_POINT('Ctrl Pts',(-1.97289186263272,-1.,0.486502692907659));
#21976=CARTESIAN_POINT('Ctrl Pts',(-1.96792703422362,-1.,0.48290166212069));
#21977=CARTESIAN_POINT('Ctrl Pts',(-1.96294933055943,-1.,0.479349583074855));
#21978=CARTESIAN_POINT('Ctrl Pts',(-1.95796111148177,-1.,0.475848034683176));
#21979=CARTESIAN_POINT('Ctrl Pts',(-1.95296148278133,-1.,0.472397672264072));
#21980=CARTESIAN_POINT('Ctrl Pts',(-1.94794381136514,-1.,0.468997482913135));
#21981=CARTESIAN_POINT('Ctrl Pts',(-1.9428979419619,-1.,0.46564546202603));
#21982=CARTESIAN_POINT('Ctrl Pts',(-1.93781486640821,-1.,0.462340031009056));
#21983=CARTESIAN_POINT('Ctrl Pts',(-1.93269066517934,-1.,0.459081234547926));
#21984=CARTESIAN_POINT('Ctrl Pts',(-1.92753067150476,-1.,0.455872005174371));
#21985=CARTESIAN_POINT('Ctrl Pts',(-1.92235380648502,-1.,0.452719478359432));
#21986=CARTESIAN_POINT('Ctrl Pts',(-1.91718342555755,-1.,0.449632260106662));
#21987=CARTESIAN_POINT('Ctrl Pts',(-1.9120369998112,-1.,0.446617343485711));
#21988=CARTESIAN_POINT('Ctrl Pts',(-1.90691756144898,-1.,0.44367755684915));
#21989=CARTESIAN_POINT('Ctrl Pts',(-1.90180124389086,-1.,0.440807833704038));
#21990=CARTESIAN_POINT('Ctrl Pts',(-1.89663648956466,-1.,0.437995003948244));
#21991=CARTESIAN_POINT('Ctrl Pts',(-1.89136993975504,-1.,0.435225660963383));
#21992=CARTESIAN_POINT('Ctrl Pts',(-1.88596913666793,-1.,0.432493038548748));
#21993=CARTESIAN_POINT('Ctrl Pts',(-1.88044229001832,-1.,0.429803062482344));
#21994=CARTESIAN_POINT('Ctrl Pts',(-1.87486989291484,-1.,0.427183828519102));
#21995=CARTESIAN_POINT('Ctrl Pts',(-1.86937803944323,-1.,0.424678177291359));
#21996=CARTESIAN_POINT('Ctrl Pts',(-1.86408083334028,-1.,0.422327307418275));
#21997=CARTESIAN_POINT('Ctrl Pts',(-1.85903281096686,-1.,0.420157287975619));
#21998=CARTESIAN_POINT('Ctrl Pts',(-1.85417632856234,-1.,0.418164129143534));
#21999=CARTESIAN_POINT('Ctrl Pts',(-1.84929312929882,-1.,0.416300022038864));
#22000=CARTESIAN_POINT('Ctrl Pts',(-1.8440575707371,-1.,0.41448743825434));
#22001=CARTESIAN_POINT('Ctrl Pts',(-1.83808953475839,-1.,0.412633125322161));
#22002=CARTESIAN_POINT('Ctrl Pts',(-1.83100408895216,-1.,0.410641256301675));
#22003=CARTESIAN_POINT('Ctrl Pts',(-1.8224702267854,-1.,0.408428948108533));
#22004=CARTESIAN_POINT('Ctrl Pts',(-1.81223801813988,-1.,0.405933518411838));
#22005=CARTESIAN_POINT('Ctrl Pts',(-1.80012077176221,-1.,0.403107976170441));
#22006=CARTESIAN_POINT('Ctrl Pts',(-1.78598826347533,-1.,0.39991940378308));
#22007=CARTESIAN_POINT('Ctrl Pts',(-1.7697556004756,-1.,0.39634619612042));
#22008=CARTESIAN_POINT('Ctrl Pts',(-1.75137405313962,-1.,0.392375812294307));
#22009=CARTESIAN_POINT('Ctrl Pts',(-1.7349317097561,-1.,0.388877023509191));
#22010=CARTESIAN_POINT('Ctrl Pts',(-1.72162022246158,-1.,0.38607079032701));
#22011=CARTESIAN_POINT('Ctrl Pts',(-1.71231062891958,-1.,0.384119047315542));
#22012=CARTESIAN_POINT('Ctrl Pts',(-1.7075470150345,-1.,0.383122945602004));
#22013=CARTESIAN_POINT('',(-1.74236521665491,-1.,0.163289472382896));
#22014=CARTESIAN_POINT('Origin',(0.,-1.,0.));
#22015=CARTESIAN_POINT('',(-2.19890268624765,-1.,0.069476445021958));
#22016=CARTESIAN_POINT('Ctrl Pts',(-1.74236521665491,-1.,0.163289472382896));
#22017=CARTESIAN_POINT('Ctrl Pts',(-1.7472034950333,-1.,0.163814161002002));
#22018=CARTESIAN_POINT('Ctrl Pts',(-1.75666056638427,-1.,0.164834765707158));
#22019=CARTESIAN_POINT('Ctrl Pts',(-1.77018771684844,-1.,0.1662793551464));
#22020=CARTESIAN_POINT('Ctrl Pts',(-1.7869064998507,-1.,0.168032772805197));
#22021=CARTESIAN_POINT('Ctrl Pts',(-1.80561530629706,-1.,0.169936923904608));
#22022=CARTESIAN_POINT('Ctrl Pts',(-1.82215766811545,-1.,0.171554770204119));
#22023=CARTESIAN_POINT('Ctrl Pts',(-1.83658380527692,-1.,0.1728894428919));
#22024=CARTESIAN_POINT('Ctrl Pts',(-1.8489811319852,-1.,0.173946627587731));
#22025=CARTESIAN_POINT('Ctrl Pts',(-1.85948367088837,-1.,0.17473525927603));
#22026=CARTESIAN_POINT('Ctrl Pts',(-1.86828349694799,-1.,0.175268337590758));
#22027=CARTESIAN_POINT('Ctrl Pts',(-1.87563767773588,-1.,0.175563480746485));
#22028=CARTESIAN_POINT('Ctrl Pts',(-1.88188663145367,-1.,0.175644148889698));
#22029=CARTESIAN_POINT('Ctrl Pts',(-1.88742606273259,-1.,0.175538155840648));
#22030=CARTESIAN_POINT('Ctrl Pts',(-1.892646301985,-1.,0.175274276190844));
#22031=CARTESIAN_POINT('Ctrl Pts',(-1.89788101117132,-1.,0.174879405091263));
#22032=CARTESIAN_POINT('Ctrl Pts',(-1.90335253862834,-1.,0.174375518661085));
#22033=CARTESIAN_POINT('Ctrl Pts',(-1.90911693975267,-1.,0.173776635257817));
#22034=CARTESIAN_POINT('Ctrl Pts',(-1.91511429159527,-1.,0.173090695383496));
#22035=CARTESIAN_POINT('Ctrl Pts',(-1.9212233439798,-1.,0.172321621259514));
#22036=CARTESIAN_POINT('Ctrl Pts',(-1.92731093582036,-1.,0.171471191532988));
#22037=CARTESIAN_POINT('Ctrl Pts',(-1.93329183155539,-1.,0.170541253116201));
#22038=CARTESIAN_POINT('Ctrl Pts',(-1.93915639211581,-1.,0.169534904817491));
#22039=CARTESIAN_POINT('Ctrl Pts',(-1.94493757756931,-1.,0.168455741607556));
#22040=CARTESIAN_POINT('Ctrl Pts',(-1.95069027794294,-1.,0.167307501784475));
#22041=CARTESIAN_POINT('Ctrl Pts',(-1.9564675971873,-1.,0.166093592002812));
#22042=CARTESIAN_POINT('Ctrl Pts',(-1.96229379940136,-1.,0.164816568920269));
#22043=CARTESIAN_POINT('Ctrl Pts',(-1.96816512677967,-1.,0.163478185457734));
#22044=CARTESIAN_POINT('Ctrl Pts',(-1.97406280235188,-1.,0.162079693556288));
#22045=CARTESIAN_POINT('Ctrl Pts',(-1.97996195437559,-1.,0.160622060784611));
#22046=CARTESIAN_POINT('Ctrl Pts',(-1.98584238283292,-1.,0.159106226437299));
#22047=CARTESIAN_POINT('Ctrl Pts',(-1.99169810931908,-1.,0.157533331459227));
#22048=CARTESIAN_POINT('Ctrl Pts',(-1.99753284771497,-1.,0.155904629548783));
#22049=CARTESIAN_POINT('Ctrl Pts',(-2.00335565310543,-1.,0.154221403049722));
#22050=CARTESIAN_POINT('Ctrl Pts',(-2.00917680318424,-1.,0.15248488362145));
#22051=CARTESIAN_POINT('Ctrl Pts',(-2.01500291940238,-1.,0.150696157673078));
#22052=CARTESIAN_POINT('Ctrl Pts',(-2.02083464969894,-1.,0.148856124775337));
#22053=CARTESIAN_POINT('Ctrl Pts',(-2.02666926182017,-1.,0.146965557332583));
#22054=CARTESIAN_POINT('Ctrl Pts',(-2.03250223739942,-1.,0.145025140186057));
#22055=CARTESIAN_POINT('Ctrl Pts',(-2.03832911025912,-1.,0.143035515058209));
#22056=CARTESIAN_POINT('Ctrl Pts',(-2.04414757947916,-1.,0.140997332152546));
#22057=CARTESIAN_POINT('Ctrl Pts',(-2.04995762001328,-1.,0.138911255368966));
#22058=CARTESIAN_POINT('Ctrl Pts',(-2.05576044414264,-1.,0.136777941218043));
#22059=CARTESIAN_POINT('Ctrl Pts',(-2.06155781517842,-1.,0.134598026192106));
#22060=CARTESIAN_POINT('Ctrl Pts',(-2.06735123910326,-1.,0.13237211154771));
#22061=CARTESIAN_POINT('Ctrl Pts',(-2.07314114713063,-1.,0.130100748328403));
#22062=CARTESIAN_POINT('Ctrl Pts',(-2.07892715110987,-1.,0.12778444527612));
#22063=CARTESIAN_POINT('Ctrl Pts',(-2.08470840653643,-1.,0.125423679412061));
#22064=CARTESIAN_POINT('Ctrl Pts',(-2.09048392424825,-1.,0.123018905621083));
#22065=CARTESIAN_POINT('Ctrl Pts',(-2.0962529286773,-1.,0.120570567965122));
#22066=CARTESIAN_POINT('Ctrl Pts',(-2.102015121329,-1.,0.118079107988355));
#22067=CARTESIAN_POINT('Ctrl Pts',(-2.10777050261309,-1.,0.115544957687926));
#22068=CARTESIAN_POINT('Ctrl Pts',(-2.11351924490306,-1.,0.112968534419737));
#22069=CARTESIAN_POINT('Ctrl Pts',(-2.11926155590865,-1.,0.110350236135025));
#22070=CARTESIAN_POINT('Ctrl Pts',(-2.12499752307,-1.,0.10769043523109));
#22071=CARTESIAN_POINT('Ctrl Pts',(-2.13072704887293,-1.,0.104989479152739));
#22072=CARTESIAN_POINT('Ctrl Pts',(-2.13644992667165,-1.,0.1022477005561));
#22073=CARTESIAN_POINT('Ctrl Pts',(-2.14216588396025,-1.,0.0994654261990914));
#22074=CARTESIAN_POINT('Ctrl Pts',(-2.14787463531795,-1.,0.0966429852305457));
#22075=CARTESIAN_POINT('Ctrl Pts',(-2.1535759397817,-1.,0.0937807218867642));
#22076=CARTESIAN_POINT('Ctrl Pts',(-2.15926961544516,-1.,0.0908789888107264));
#22077=CARTESIAN_POINT('Ctrl Pts',(-2.16495552645014,-1.,0.0879381291386921));
#22078=CARTESIAN_POINT('Ctrl Pts',(-2.17063357870952,-1.,0.0849584620835371));
#22079=CARTESIAN_POINT('Ctrl Pts',(-2.176303712113,-1.,0.0819402680872764));
#22080=CARTESIAN_POINT('Ctrl Pts',(-2.18196589448887,-1.,0.0788837727685241));
#22081=CARTESIAN_POINT('Ctrl Pts',(-2.1876201139953,-1.,0.0757891465836146));
#22082=CARTESIAN_POINT('Ctrl Pts',(-2.19213712013662,-1.,0.0732830357306724));
#22083=CARTESIAN_POINT('Ctrl Pts',(-2.19552129484002,-1.,0.0713863779526153));
#22084=CARTESIAN_POINT('Ctrl Pts',(-2.19777582085423,-1.,0.0701143536325489));
#22085=CARTESIAN_POINT('Ctrl Pts',(-2.19890268624765,-1.,0.069476445021958));
#22086=CARTESIAN_POINT('',(-2.19890268624765,-1.,-0.0694764450219585));
#22087=CARTESIAN_POINT('',(-2.19890268624765,-1.,0.069476445021958));
#22088=CARTESIAN_POINT('',(-1.74236521665491,-1.,-0.163289472382896));
#22089=CARTESIAN_POINT('Ctrl Pts',(-2.19890268624765,-1.,-0.0694764450219585));
#22090=CARTESIAN_POINT('Ctrl Pts',(-2.19777582085261,-1.,-0.0701143536324927));
#22091=CARTESIAN_POINT('Ctrl Pts',(-2.19552129483562,-1.,-0.0713863779524629));
#22092=CARTESIAN_POINT('Ctrl Pts',(-2.19213712012956,-1.,-0.0732830357304277));
#22093=CARTESIAN_POINT('Ctrl Pts',(-2.1876201139874,-1.,-0.0757891465833413));
#22094=CARTESIAN_POINT('Ctrl Pts',(-2.18196589448304,-1.,-0.0788837727683229));
#22095=CARTESIAN_POINT('Ctrl Pts',(-2.1763037121106,-1.,-0.0819402680871941));
#22096=CARTESIAN_POINT('Ctrl Pts',(-2.17063357871031,-1.,-0.0849584620835644));
#22097=CARTESIAN_POINT('Ctrl Pts',(-2.16495552645275,-1.,-0.0879381291387824));
#22098=CARTESIAN_POINT('Ctrl Pts',(-2.15926961544808,-1.,-0.0908789888108267));
#22099=CARTESIAN_POINT('Ctrl Pts',(-2.15357593978377,-1.,-0.0937807218868346));
#22100=CARTESIAN_POINT('Ctrl Pts',(-2.14787463531864,-1.,-0.096642985230569));
#22101=CARTESIAN_POINT('Ctrl Pts',(-2.14216588395974,-1.,-0.0994654261990744));
#22102=CARTESIAN_POINT('Ctrl Pts',(-2.13644992667052,-1.,-0.102247700556064));
#22103=CARTESIAN_POINT('Ctrl Pts',(-2.1307270488718,-1.,-0.104989479152703));
#22104=CARTESIAN_POINT('Ctrl Pts',(-2.12499752306927,-1.,-0.107690435231068));
#22105=CARTESIAN_POINT('Ctrl Pts',(-2.11926155590849,-1.,-0.11035023613502));
#22106=CARTESIAN_POINT('Ctrl Pts',(-2.11351924490335,-1.,-0.112968534419746));
#22107=CARTESIAN_POINT('Ctrl Pts',(-2.10777050261359,-1.,-0.11554495768794));
#22108=CARTESIAN_POINT('Ctrl Pts',(-2.10201512132945,-1.,-0.118079107988368));
#22109=CARTESIAN_POINT('Ctrl Pts',(-2.09625292867756,-1.,-0.120570567965129));
#22110=CARTESIAN_POINT('Ctrl Pts',(-2.09048392424826,-1.,-0.123018905621083));
#22111=CARTESIAN_POINT('Ctrl Pts',(-2.08470840653628,-1.,-0.125423679412058));
#22112=CARTESIAN_POINT('Ctrl Pts',(-2.07892715110967,-1.,-0.127784445276116));
#22113=CARTESIAN_POINT('Ctrl Pts',(-2.07314114713047,-1.,-0.130100748328401));
#22114=CARTESIAN_POINT('Ctrl Pts',(-2.06735123910319,-1.,-0.13237211154771));
#22115=CARTESIAN_POINT('Ctrl Pts',(-2.06155781517844,-1.,-0.134598026192107));
#22116=CARTESIAN_POINT('Ctrl Pts',(-2.0557604441427,-1.,-0.136777941218044));
#22117=CARTESIAN_POINT('Ctrl Pts',(-2.04995762001333,-1.,-0.138911255368966));
#22118=CARTESIAN_POINT('Ctrl Pts',(-2.04414757947919,-1.,-0.140997332152545));
#22119=CARTESIAN_POINT('Ctrl Pts',(-2.03832911025913,-1.,-0.143035515058208));
#22120=CARTESIAN_POINT('Ctrl Pts',(-2.03250223739941,-1.,-0.145025140186058));
#22121=CARTESIAN_POINT('Ctrl Pts',(-2.02666926182017,-1.,-0.146965557332586));
#22122=CARTESIAN_POINT('Ctrl Pts',(-2.02083464969897,-1.,-0.148856124775343));
#22123=CARTESIAN_POINT('Ctrl Pts',(-2.01500291940243,-1.,-0.150696157673084));
#22124=CARTESIAN_POINT('Ctrl Pts',(-2.00917680318426,-1.,-0.152484883621452));
#22125=CARTESIAN_POINT('Ctrl Pts',(-2.00335565310539,-1.,-0.154221403049719));
#22126=CARTESIAN_POINT('Ctrl Pts',(-1.99753284771487,-1.,-0.155904629548775));
#22127=CARTESIAN_POINT('Ctrl Pts',(-1.99169810931893,-1.,-0.157533331459215));
#22128=CARTESIAN_POINT('Ctrl Pts',(-1.98584238283279,-1.,-0.159106226437289));
#22129=CARTESIAN_POINT('Ctrl Pts',(-1.97996195437557,-1.,-0.16062206078461));
#22130=CARTESIAN_POINT('Ctrl Pts',(-1.97406280235204,-1.,-0.162079693556302));
#22131=CARTESIAN_POINT('Ctrl Pts',(-1.96816512678,-1.,-0.16347818545776));
#22132=CARTESIAN_POINT('Ctrl Pts',(-1.96229379940174,-1.,-0.1648165689203));
#22133=CARTESIAN_POINT('Ctrl Pts',(-1.95646759718755,-1.,-0.166093592002833));
#22134=CARTESIAN_POINT('Ctrl Pts',(-1.95069027794286,-1.,-0.167307501784469));
#22135=CARTESIAN_POINT('Ctrl Pts',(-1.94493757756879,-1.,-0.168455741607516));
#22136=CARTESIAN_POINT('Ctrl Pts',(-1.93915639211497,-1.,-0.169534904817425));
#22137=CARTESIAN_POINT('Ctrl Pts',(-1.93329183155455,-1.,-0.170541253116136));
#22138=CARTESIAN_POINT('Ctrl Pts',(-1.92731093582,-1.,-0.17147119153296));
#22139=CARTESIAN_POINT('Ctrl Pts',(-1.92122334398034,-1.,-0.172321621259557));
#22140=CARTESIAN_POINT('Ctrl Pts',(-1.91511429159681,-1.,-0.173090695383619));
#22141=CARTESIAN_POINT('Ctrl Pts',(-1.90911693975475,-1.,-0.173776635257984));
#22142=CARTESIAN_POINT('Ctrl Pts',(-1.90335253863003,-1.,-0.174375518661222));
#22143=CARTESIAN_POINT('Ctrl Pts',(-1.89788101117148,-1.,-0.174879405091277));
#22144=CARTESIAN_POINT('Ctrl Pts',(-1.89264630198279,-1.,-0.175274276190664));
#22145=CARTESIAN_POINT('Ctrl Pts',(-1.88742606272818,-1.,-0.175538155840286));
#22146=CARTESIAN_POINT('Ctrl Pts',(-1.88188663144846,-1.,-0.175644148889271));
#22147=CARTESIAN_POINT('Ctrl Pts',(-1.87563767773249,-1.,-0.175563480746205));
#22148=CARTESIAN_POINT('Ctrl Pts',(-1.86828349694972,-1.,-0.175268337590901));
#22149=CARTESIAN_POINT('Ctrl Pts',(-1.85948367089838,-1.,-0.174735259276856));
#22150=CARTESIAN_POINT('Ctrl Pts',(-1.84898113200543,-1.,-0.173946627589401));
#22151=CARTESIAN_POINT('Ctrl Pts',(-1.83658380530747,-1.,-0.17288944289442));
#22152=CARTESIAN_POINT('Ctrl Pts',(-1.82215766815414,-1.,-0.171554770207306));
#22153=CARTESIAN_POINT('Ctrl Pts',(-1.80561530633924,-1.,-0.169936923908078));
#22154=CARTESIAN_POINT('Ctrl Pts',(-1.78690649988931,-1.,-0.16803277280837));
#22155=CARTESIAN_POINT('Ctrl Pts',(-1.77018771687692,-1.,-0.166279355148738));
#22156=CARTESIAN_POINT('Ctrl Pts',(-1.75666056640041,-1.,-0.164834765708484));
#22157=CARTESIAN_POINT('Ctrl Pts',(-1.74720349503904,-1.,-0.163814161002474));
#22158=CARTESIAN_POINT('Ctrl Pts',(-1.74236521665491,-1.,-0.163289472382896));
#22159=CARTESIAN_POINT('',(-1.7075470150345,-1.,-0.383122945602004));
#22160=CARTESIAN_POINT('Origin',(0.,-1.,0.));
#22161=CARTESIAN_POINT('',(-2.11275013067528,-1.,-0.61342227326009));
#22162=CARTESIAN_POINT('Ctrl Pts',(-1.7075470150345,-1.,-0.383122945602004));
#22163=CARTESIAN_POINT('Ctrl Pts',(-1.71231062891398,-1.,-0.384119047314215));
#22164=CARTESIAN_POINT('Ctrl Pts',(-1.72162022244582,-1.,-0.386070790323281));
#22165=CARTESIAN_POINT('Ctrl Pts',(-1.73493170972829,-1.,-0.388877023502615));
#22166=CARTESIAN_POINT('Ctrl Pts',(-1.75137405310193,-1.,-0.392375812285395));
#22167=CARTESIAN_POINT('Ctrl Pts',(-1.76975560043442,-1.,-0.396346196110688));
#22168=CARTESIAN_POINT('Ctrl Pts',(-1.78598826343754,-1.,-0.399919403774155));
#22169=CARTESIAN_POINT('Ctrl Pts',(-1.80012077173238,-1.,-0.403107976163396));
#22170=CARTESIAN_POINT('Ctrl Pts',(-1.81223801812013,-1.,-0.405933518407175));
#22171=CARTESIAN_POINT('Ctrl Pts',(-1.82247022677562,-1.,-0.408428948106227));
#22172=CARTESIAN_POINT('Ctrl Pts',(-1.83100408895047,-1.,-0.410641256301276));
#22173=CARTESIAN_POINT('Ctrl Pts',(-1.8380895347617,-1.,-0.412633125322945));
#22174=CARTESIAN_POINT('Ctrl Pts',(-1.84405757074218,-1.,-0.414487438255542));
#22175=CARTESIAN_POINT('Ctrl Pts',(-1.84929312930314,-1.,-0.416300022039885));
#22176=CARTESIAN_POINT('Ctrl Pts',(-1.8541763285645,-1.,-0.418164129144045));
#22177=CARTESIAN_POINT('Ctrl Pts',(-1.8590328109667,-1.,-0.420157287975583));
#22178=CARTESIAN_POINT('Ctrl Pts',(-1.86408083333863,-1.,-0.422327307417884));
#22179=CARTESIAN_POINT('Ctrl Pts',(-1.8693780394412,-1.,-0.424678177290876));
#22180=CARTESIAN_POINT('Ctrl Pts',(-1.87486989291333,-1.,-0.427183828518743));
#22181=CARTESIAN_POINT('Ctrl Pts',(-1.88044229001778,-1.,-0.429803062482217));
#22182=CARTESIAN_POINT('Ctrl Pts',(-1.88596913666828,-1.,-0.432493038548833));
#22183=CARTESIAN_POINT('Ctrl Pts',(-1.89136993975585,-1.,-0.43522566096358));
#22184=CARTESIAN_POINT('Ctrl Pts',(-1.89663648956549,-1.,-0.437995003948443));
#22185=CARTESIAN_POINT('Ctrl Pts',(-1.90180124389137,-1.,-0.44080783370416));
#22186=CARTESIAN_POINT('Ctrl Pts',(-1.90691756144906,-1.,-0.44367755684917));
#22187=CARTESIAN_POINT('Ctrl Pts',(-1.91203699981095,-1.,-0.446617343485651));
#22188=CARTESIAN_POINT('Ctrl Pts',(-1.91718342555717,-1.,-0.449632260106572));
#22189=CARTESIAN_POINT('Ctrl Pts',(-1.9223538064847,-1.,-0.452719478359356));
#22190=CARTESIAN_POINT('Ctrl Pts',(-1.92753067150461,-1.,-0.455872005174335));
#22191=CARTESIAN_POINT('Ctrl Pts',(-1.93269066517936,-1.,-0.459081234547931));
#22192=CARTESIAN_POINT('Ctrl Pts',(-1.93781486640834,-1.,-0.462340031009087));
#22193=CARTESIAN_POINT('Ctrl Pts',(-1.94289794196205,-1.,-0.465645462026064));
#22194=CARTESIAN_POINT('Ctrl Pts',(-1.94794381136524,-1.,-0.468997482913158));
#22195=CARTESIAN_POINT('Ctrl Pts',(-1.95296148278136,-1.,-0.472397672264079));
#22196=CARTESIAN_POINT('Ctrl Pts',(-1.95796111148175,-1.,-0.475848034683171));
#22197=CARTESIAN_POINT('Ctrl Pts',(-1.96294933055938,-1.,-0.479349583074846));
#22198=CARTESIAN_POINT('Ctrl Pts',(-1.96792703422358,-1.,-0.482901662120686));
#22199=CARTESIAN_POINT('Ctrl Pts',(-1.97289186263272,-1.,-0.486502692907661));
#22200=CARTESIAN_POINT('Ctrl Pts',(-1.97783973019229,-1.,-0.490150627860955));
#22201=CARTESIAN_POINT('Ctrl Pts',(-1.9827665876182,-1.,-0.493843476541492));
#22202=CARTESIAN_POINT('Ctrl Pts',(-1.98767044752929,-1.,-0.497579909545564));
#22203=CARTESIAN_POINT('Ctrl Pts',(-1.9925514912615,-1.,-0.501359287727129));
#22204=CARTESIAN_POINT('Ctrl Pts',(-1.99741107463567,-1.,-0.505181361323011));
#22205=CARTESIAN_POINT('Ctrl Pts',(-2.00225107134733,-1.,-0.509046069886152));
#22206=CARTESIAN_POINT('Ctrl Pts',(-2.00707309946955,-1.,-0.512953306961813));
#22207=CARTESIAN_POINT('Ctrl Pts',(-2.01187773939257,-1.,-0.516902681728733));
#22208=CARTESIAN_POINT('Ctrl Pts',(-2.01666477917305,-1.,-0.520893590399428));
#22209=CARTESIAN_POINT('Ctrl Pts',(-2.02143356304712,-1.,-0.524925318333518));
#22210=CARTESIAN_POINT('Ctrl Pts',(-2.02618329083289,-1.,-0.52899712724191));
#22211=CARTESIAN_POINT('Ctrl Pts',(-2.03091336214401,-1.,-0.533108355132905));
#22212=CARTESIAN_POINT('Ctrl Pts',(-2.03562362953993,-1.,-0.537258489833134));
#22213=CARTESIAN_POINT('Ctrl Pts',(-2.0403142269048,-1.,-0.54144712061552));
#22214=CARTESIAN_POINT('Ctrl Pts',(-2.0449854471456,-1.,-0.545673903817348));
#22215=CARTESIAN_POINT('Ctrl Pts',(-2.04963761077974,-1.,-0.549938525150342));
#22216=CARTESIAN_POINT('Ctrl Pts',(-2.05427091604482,-1.,-0.554240657464109));
#22217=CARTESIAN_POINT('Ctrl Pts',(-2.05888537756571,-1.,-0.558579940185467));
#22218=CARTESIAN_POINT('Ctrl Pts',(-2.06348090160697,-1.,-0.562955993082574));
#22219=CARTESIAN_POINT('Ctrl Pts',(-2.06805732997383,-1.,-0.567368421181229));
#22220=CARTESIAN_POINT('Ctrl Pts',(-2.07261449292757,-1.,-0.571816823242411));
#22221=CARTESIAN_POINT('Ctrl Pts',(-2.07715226767361,-1.,-0.576300797416274));
#22222=CARTESIAN_POINT('Ctrl Pts',(-2.08167059018138,-1.,-0.580819952107257));
#22223=CARTESIAN_POINT('Ctrl Pts',(-2.086169437277,-1.,-0.585373918990895));
#22224=CARTESIAN_POINT('Ctrl Pts',(-2.09064881812053,-1.,-0.589962365403189));
#22225=CARTESIAN_POINT('Ctrl Pts',(-2.09510876220501,-1.,-0.594585006052823));
#22226=CARTESIAN_POINT('Ctrl Pts',(-2.09954930865331,-1.,-0.599241616422144));
#22227=CARTESIAN_POINT('Ctrl Pts',(-2.10397049887709,-1.,-0.603932030738212));
#22228=CARTESIAN_POINT('Ctrl Pts',(-2.10749199615859,-1.,-0.607711315456826));
#22229=CARTESIAN_POINT('Ctrl Pts',(-2.11012443807661,-1.,-0.610560911691113));
#22230=CARTESIAN_POINT('Ctrl Pts',(-2.11187554260142,-1.,-0.61246736556225));
#22231=CARTESIAN_POINT('Ctrl Pts',(-2.11275013067528,-1.,-0.61342227326009));
#22232=CARTESIAN_POINT('',(-2.0698113262342,-1.,-0.745574324794401));
#22233=CARTESIAN_POINT('',(-2.11275013067528,-1.,-0.61342227326009));
#22234=CARTESIAN_POINT('',(-1.60662857109684,-1.,-0.693717979106306));
#22235=CARTESIAN_POINT('Ctrl Pts',(-2.0698113262342,-1.,-0.745574324794401));
#22236=CARTESIAN_POINT('Ctrl Pts',(-2.06854248895575,-1.,-0.74583279137781));
#22237=CARTESIAN_POINT('Ctrl Pts',(-2.06600523016401,-1.,-0.746345871542695));
#22238=CARTESIAN_POINT('Ctrl Pts',(-2.06220058927162,-1.,-0.747103932785504));
#22239=CARTESIAN_POINT('Ctrl Pts',(-2.05713023030263,-1.,-0.748091554181101));
#22240=CARTESIAN_POINT('Ctrl Pts',(-2.05079645591606,-1.,-0.749287468663053));
#22241=CARTESIAN_POINT('Ctrl Pts',(-2.04446689147754,-1.,-0.750444657874758));
#22242=CARTESIAN_POINT('Ctrl Pts',(-2.03814160092173,-1.,-0.751562963361383));
#22243=CARTESIAN_POINT('Ctrl Pts',(-2.03182068456467,-1.,-0.752642180488104));
#22244=CARTESIAN_POINT('Ctrl Pts',(-2.02550428623587,-1.,-0.753682061113765));
#22245=CARTESIAN_POINT('Ctrl Pts',(-2.01919259406003,-1.,-0.75468233072352));
#22246=CARTESIAN_POINT('Ctrl Pts',(-2.01288584328149,-1.,-0.7556427049581));
#22247=CARTESIAN_POINT('Ctrl Pts',(-2.00658431587682,-1.,-0.756562904646496));
#22248=CARTESIAN_POINT('Ctrl Pts',(-2.00028834739072,-1.,-0.757442676862341));
#22249=CARTESIAN_POINT('Ctrl Pts',(-1.9939983109871,-1.,-0.758281796766377));
#22250=CARTESIAN_POINT('Ctrl Pts',(-1.98771456680806,-1.,-0.759080037802242));
#22251=CARTESIAN_POINT('Ctrl Pts',(-1.98143741418156,-1.,-0.759837147452135));
#22252=CARTESIAN_POINT('Ctrl Pts',(-1.97516705321521,-1.,-0.760552825409855));
#22253=CARTESIAN_POINT('Ctrl Pts',(-1.96890351582545,-1.,-0.761226690483986));
#22254=CARTESIAN_POINT('Ctrl Pts',(-1.96264672744229,-1.,-0.761858300014575));
#22255=CARTESIAN_POINT('Ctrl Pts',(-1.95639665309893,-1.,-0.762447203806263));
#22256=CARTESIAN_POINT('Ctrl Pts',(-1.95015342590025,-1.,-0.762992990878774));
#22257=CARTESIAN_POINT('Ctrl Pts',(-1.94391746617626,-1.,-0.76349533353858));
#22258=CARTESIAN_POINT('Ctrl Pts',(-1.93768964875867,-1.,-0.763954049121393));
#22259=CARTESIAN_POINT('Ctrl Pts',(-1.93147105496367,-1.,-0.764369010673889));
#22260=CARTESIAN_POINT('Ctrl Pts',(-1.92526263537041,-1.,-0.764740025488189));
#22261=CARTESIAN_POINT('Ctrl Pts',(-1.91906491634197,-1.,-0.765066729667095));
#22262=CARTESIAN_POINT('Ctrl Pts',(-1.91287765805174,-1.,-0.765348465884739));
#22263=CARTESIAN_POINT('Ctrl Pts',(-1.90669961402362,-1.,-0.765584196937936));
#22264=CARTESIAN_POINT('Ctrl Pts',(-1.90052930393599,-1.,-0.765772772593395));
#22265=CARTESIAN_POINT('Ctrl Pts',(-1.89436577771389,-1.,-0.765913193856979));
#22266=CARTESIAN_POINT('Ctrl Pts',(-1.88820926433409,-1.,-0.76600483706209));
#22267=CARTESIAN_POINT('Ctrl Pts',(-1.88206215302561,-1.,-0.766047794851868));
#22268=CARTESIAN_POINT('Ctrl Pts',(-1.87592888967886,-1.,-0.766042837036759));
#22269=CARTESIAN_POINT('Ctrl Pts',(-1.86981398314345,-1.,-0.765990708546111));
#22270=CARTESIAN_POINT('Ctrl Pts',(-1.86372027063314,-1.,-0.765891519092557));
#22271=CARTESIAN_POINT('Ctrl Pts',(-1.85764741390391,-1.,-0.765744212909305));
#22272=CARTESIAN_POINT('Ctrl Pts',(-1.85158945130054,-1.,-0.765545710619023));
#22273=CARTESIAN_POINT('Ctrl Pts',(-1.8455369887591,-1.,-0.765291664861971));
#22274=CARTESIAN_POINT('Ctrl Pts',(-1.83948181064823,-1.,-0.764978057881687));
#22275=CARTESIAN_POINT('Ctrl Pts',(-1.8334207722714,-1.,-0.764602549687845));
#22276=CARTESIAN_POINT('Ctrl Pts',(-1.8273599120008,-1.,-0.764165902606055));
#22277=CARTESIAN_POINT('Ctrl Pts',(-1.82131873145297,-1.,-0.763673465462854));
#22278=CARTESIAN_POINT('Ctrl Pts',(-1.81532118405566,-1.,-0.763132003836783));
#22279=CARTESIAN_POINT('Ctrl Pts',(-1.80938551463989,-1.,-0.762546129464036));
#22280=CARTESIAN_POINT('Ctrl Pts',(-1.80351583877334,-1.,-0.761915336443515));
#22281=CARTESIAN_POINT('Ctrl Pts',(-1.79768986997735,-1.,-0.761229695230359));
#22282=CARTESIAN_POINT('Ctrl Pts',(-1.79185815610802,-1.,-0.760469555880425));
#22283=CARTESIAN_POINT('Ctrl Pts',(-1.78596964884526,-1.,-0.759614401109868));
#22284=CARTESIAN_POINT('Ctrl Pts',(-1.77999411220912,-1.,-0.75865062667738));
#22285=CARTESIAN_POINT('Ctrl Pts',(-1.77394167108342,-1.,-0.757578264077238));
#22286=CARTESIAN_POINT('Ctrl Pts',(-1.76789396003141,-1.,-0.756421896028403));
#22287=CARTESIAN_POINT('Ctrl Pts',(-1.7619781724032,-1.,-0.755220979975262));
#22288=CARTESIAN_POINT('Ctrl Pts',(-1.75631083600175,-1.,-0.75400925402848));
#22289=CARTESIAN_POINT('Ctrl Pts',(-1.75095139468809,-1.,-0.752797683531377));
#22290=CARTESIAN_POINT('Ctrl Pts',(-1.74585086852298,-1.,-0.751555614163629));
#22291=CARTESIAN_POINT('Ctrl Pts',(-1.74080458266705,-1.,-0.75019343597954));
#22292=CARTESIAN_POINT('Ctrl Pts',(-1.73550351679848,-1.,-0.748582462954854));
#22293=CARTESIAN_POINT('Ctrl Pts',(-1.72958533647399,-1.,-0.746574710096436));
#22294=CARTESIAN_POINT('Ctrl Pts',(-1.7226822991693,-1.,-0.744021445433764));
#22295=CARTESIAN_POINT('Ctrl Pts',(-1.71447789751927,-1.,-0.740795162032087));
#22296=CARTESIAN_POINT('Ctrl Pts',(-1.70473309006121,-1.,-0.736799665724771));
#22297=CARTESIAN_POINT('Ctrl Pts',(-1.69326921975743,-1.,-0.731963238697195));
#22298=CARTESIAN_POINT('Ctrl Pts',(-1.67996158455503,-1.,-0.726235967997433));
#22299=CARTESIAN_POINT('Ctrl Pts',(-1.6647288055568,-1.,-0.719585433804282));
#22300=CARTESIAN_POINT('Ctrl Pts',(-1.64752408832016,-1.,-0.711993139355394));
#22301=CARTESIAN_POINT('Ctrl Pts',(-1.63216541664676,-1.,-0.705159151988319));
#22302=CARTESIAN_POINT('Ctrl Pts',(-1.61974673472612,-1.,-0.699605146405088));
#22303=CARTESIAN_POINT('Ctrl Pts',(-1.61106790958151,-1.,-0.695712097881194));
#22304=CARTESIAN_POINT('Ctrl Pts',(-1.60662857109684,-1.,-0.693717979106306));
#22305=CARTESIAN_POINT('',(-1.5055822144029,-1.,-0.892032620296855));
#22306=CARTESIAN_POINT('Origin',(0.,-1.,0.));
#22307=CARTESIAN_POINT('',(-1.81978687191668,-1.,-1.23627494547115));
#22308=CARTESIAN_POINT('Ctrl Pts',(-1.5055822144029,-1.,-0.892032620296855));
#22309=CARTESIAN_POINT('Ctrl Pts',(-1.50980486806688,-1.,-0.894452006964543));
#22310=CARTESIAN_POINT('Ctrl Pts',(-1.51805569590094,-1.,-0.899185047483511));
#22311=CARTESIAN_POINT('Ctrl Pts',(-1.52984849887993,-1.,-0.905967409625651));
#22312=CARTESIAN_POINT('Ctrl Pts',(-1.54440491149498,-1.,-0.914375919026456));
#22313=CARTESIAN_POINT('Ctrl Pts',(-1.56065988578893,-1.,-0.923832188944341));
#22314=CARTESIAN_POINT('Ctrl Pts',(-1.57499388382243,-1.,-0.932246680108685));
#22315=CARTESIAN_POINT('Ctrl Pts',(-1.58744937487176,-1.,-0.939646377893399));
#22316=CARTESIAN_POINT('Ctrl Pts',(-1.59810042043673,-1.,-0.946078063315257));
#22317=CARTESIAN_POINT('Ctrl Pts',(-1.60706069896936,-1.,-0.951613284356035));
#22318=CARTESIAN_POINT('Ctrl Pts',(-1.61449324337085,-1.,-0.956354422920671));
#22319=CARTESIAN_POINT('Ctrl Pts',(-1.62061638140221,-1.,-0.960438326101729));
#22320=CARTESIAN_POINT('Ctrl Pts',(-1.62571930670187,-1.,-0.964046107040536));
#22321=CARTESIAN_POINT('Ctrl Pts',(-1.63013849959461,-1.,-0.967387853230345));
#22322=CARTESIAN_POINT('Ctrl Pts',(-1.63420665729798,-1.,-0.970669715997509));
#22323=CARTESIAN_POINT('Ctrl Pts',(-1.63820952658144,-1.,-0.974066058287418));
#22324=CARTESIAN_POINT('Ctrl Pts',(-1.64233990826687,-1.,-0.977689794119416));
#22325=CARTESIAN_POINT('Ctrl Pts',(-1.64665139190656,-1.,-0.981562530939489));
#22326=CARTESIAN_POINT('Ctrl Pts',(-1.65110016612638,-1.,-0.985642622920821));
#22327=CARTESIAN_POINT('Ctrl Pts',(-1.65559044289699,-1.,-0.989855627854165));
#22328=CARTESIAN_POINT('Ctrl Pts',(-1.66001553809947,-1.,-0.994121836661306));
#22329=CARTESIAN_POINT('Ctrl Pts',(-1.66430758030376,-1.,-0.998389654952758));
#22330=CARTESIAN_POINT('Ctrl Pts',(-1.66846059277303,-1.,-1.00265091003727));
#22331=CARTESIAN_POINT('Ctrl Pts',(-1.67250335383293,-1.,-1.00692206696414));
#22332=CARTESIAN_POINT('Ctrl Pts',(-1.67648246776464,-1.,-1.01123236493511));
#22333=CARTESIAN_POINT('Ctrl Pts',(-1.68044289894798,-1.,-1.01561026162773));
#22334=CARTESIAN_POINT('Ctrl Pts',(-1.68440578021706,-1.,-1.02006795074201));
#22335=CARTESIAN_POINT('Ctrl Pts',(-1.68836910178447,-1.,-1.02460180535255));
#22336=CARTESIAN_POINT('Ctrl Pts',(-1.69231840863458,-1.,-1.02919977579147));
#22337=CARTESIAN_POINT('Ctrl Pts',(-1.69623414782771,-1.,-1.03384646003588));
#22338=CARTESIAN_POINT('Ctrl Pts',(-1.70010052930962,-1.,-1.03852922490789));
#22339=CARTESIAN_POINT('Ctrl Pts',(-1.70391338707982,-1.,-1.04324363334554));
#22340=CARTESIAN_POINT('Ctrl Pts',(-1.70767646263649,-1.,-1.04799085404995));
#22341=CARTESIAN_POINT('Ctrl Pts',(-1.71139783543989,-1.,-1.05277517202855));
#22342=CARTESIAN_POINT('Ctrl Pts',(-1.7150865442702,-1.,-1.05760163192479));
#22343=CARTESIAN_POINT('Ctrl Pts',(-1.71874858456904,-1.,-1.06247324680647));
#22344=CARTESIAN_POINT('Ctrl Pts',(-1.72238500928453,-1.,-1.06738966975462));
#22345=CARTESIAN_POINT('Ctrl Pts',(-1.72599406198488,-1.,-1.07234866990252));
#22346=CARTESIAN_POINT('Ctrl Pts',(-1.72957248977424,-1.,-1.0773470373727));
#22347=CARTESIAN_POINT('Ctrl Pts',(-1.73311705663407,-1.,-1.08238162784749));
#22348=CARTESIAN_POINT('Ctrl Pts',(-1.73662628326091,-1.,-1.08745056285427));
#22349=CARTESIAN_POINT('Ctrl Pts',(-1.74010053962247,-1.,-1.09255329056493));
#22350=CARTESIAN_POINT('Ctrl Pts',(-1.74354119236208,-1.,-1.09768999241225));
#22351=CARTESIAN_POINT('Ctrl Pts',(-1.74695004214923,-1.,-1.10286118991143));
#22352=CARTESIAN_POINT('Ctrl Pts',(-1.7503286607592,-1.,-1.10806728183007));
#22353=CARTESIAN_POINT('Ctrl Pts',(-1.7536777209463,-1.,-1.11330807582551));
#22354=CARTESIAN_POINT('Ctrl Pts',(-1.75699720772105,-1.,-1.11858293216763));
#22355=CARTESIAN_POINT('Ctrl Pts',(-1.76028671825096,-1.,-1.12389096855086));
#22356=CARTESIAN_POINT('Ctrl Pts',(-1.7635457196617,-1.,-1.12923123555075));
#22357=CARTESIAN_POINT('Ctrl Pts',(-1.76677384551862,-1.,-1.1346029180462));
#22358=CARTESIAN_POINT('Ctrl Pts',(-1.76997111386769,-1.,-1.14000548336975));
#22359=CARTESIAN_POINT('Ctrl Pts',(-1.77313777896194,-1.,-1.1454385822692));
#22360=CARTESIAN_POINT('Ctrl Pts',(-1.7762742255701,-1.,-1.15090197841515));
#22361=CARTESIAN_POINT('Ctrl Pts',(-1.77938085564275,-1.,-1.15639547194698));
#22362=CARTESIAN_POINT('Ctrl Pts',(-1.78245795881009,-1.,-1.16191881298499));
#22363=CARTESIAN_POINT('Ctrl Pts',(-1.78550566040443,-1.,-1.16747166312303));
#22364=CARTESIAN_POINT('Ctrl Pts',(-1.78852398877616,-1.,-1.17305363177328));
#22365=CARTESIAN_POINT('Ctrl Pts',(-1.79151291552689,-1.,-1.17866429440809));
#22366=CARTESIAN_POINT('Ctrl Pts',(-1.79447240321515,-1.,-1.18430321697432));
#22367=CARTESIAN_POINT('Ctrl Pts',(-1.79740245923478,-1.,-1.18996997934445));
#22368=CARTESIAN_POINT('Ctrl Pts',(-1.80030314369879,-1.,-1.19566418930242));
#22369=CARTESIAN_POINT('Ctrl Pts',(-1.80317454838603,-1.,-1.20138548938974));
#22370=CARTESIAN_POINT('Ctrl Pts',(-1.80601678480707,-1.,-1.20713356605475));
#22371=CARTESIAN_POINT('Ctrl Pts',(-1.80882996917129,-1.,-1.21290815708314));
#22372=CARTESIAN_POINT('Ctrl Pts',(-1.81161420806656,-1.,-1.21870906103557));
#22373=CARTESIAN_POINT('Ctrl Pts',(-1.81436959210434,-1.,-1.2245361330495));
#22374=CARTESIAN_POINT('Ctrl Pts',(-1.8165508718364,-1.,-1.2292186489137));
#22375=CARTESIAN_POINT('Ctrl Pts',(-1.81817389921279,-1.,-1.2327422452705));
#22376=CARTESIAN_POINT('Ctrl Pts',(-1.81925017193666,-1.,-1.23509651170476));
#22377=CARTESIAN_POINT('Ctrl Pts',(-1.81978687191668,-1.,-1.23627494547115));
#22378=CARTESIAN_POINT('',(-1.73811241238545,-1.,-1.34869019493419));
#22379=CARTESIAN_POINT('',(-1.81978687191668,-1.,-1.23627494547115));
#22380=CARTESIAN_POINT('',(-1.31362392696032,-1.,-1.15624053661742));
#22381=CARTESIAN_POINT('Ctrl Pts',(-1.73811241238545,-1.,-1.34869019493419));
#22382=CARTESIAN_POINT('Ctrl Pts',(-1.73682580585691,-1.,-1.34854391898045));
#22383=CARTESIAN_POINT('Ctrl Pts',(-1.73425417885907,-1.,-1.34824783112887));
#22384=CARTESIAN_POINT('Ctrl Pts',(-1.7304014965394,-1.,-1.34779309152035));
#22385=CARTESIAN_POINT('Ctrl Pts',(-1.72527410680674,-1.,-1.34716554819527));
#22386=CARTESIAN_POINT('Ctrl Pts',(-1.7188807715049,-1.,-1.34634568653227));
#22387=CARTESIAN_POINT('Ctrl Pts',(-1.71250340686822,-1.,-1.34549029589416));
#22388=CARTESIAN_POINT('Ctrl Pts',(-1.70614212266738,-1.,-1.34459924533831));
#22389=CARTESIAN_POINT('Ctrl Pts',(-1.69979707754427,-1.,-1.34367237124483));
#22390=CARTESIAN_POINT('Ctrl Pts',(-1.6934684849687,-1.,-1.34270948206319));
#22391=CARTESIAN_POINT('Ctrl Pts',(-1.68715660868764,-1.,-1.341710374848));
#22392=CARTESIAN_POINT('Ctrl Pts',(-1.68086176030362,-1.,-1.34067485185203));
#22393=CARTESIAN_POINT('Ctrl Pts',(-1.67458429426086,-1.,-1.3396027347034));
#22394=CARTESIAN_POINT('Ctrl Pts',(-1.66832460783989,-1.,-1.33849388654388));
#22395=CARTESIAN_POINT('Ctrl Pts',(-1.66208312541983,-1.,-1.33734820885262));
#22396=CARTESIAN_POINT('Ctrl Pts',(-1.65586025952593,-1.,-1.33616559745172));
#22397=CARTESIAN_POINT('Ctrl Pts',(-1.6496563728683,-1.,-1.33494590467993));
#22398=CARTESIAN_POINT('Ctrl Pts',(-1.6434717485603,-1.,-1.33368890676572));
#22399=CARTESIAN_POINT('Ctrl Pts',(-1.63730653475089,-1.,-1.33239425103724));
#22400=CARTESIAN_POINT('Ctrl Pts',(-1.63116079730923,-1.,-1.33106149345645));
#22401=CARTESIAN_POINT('Ctrl Pts',(-1.62503464209797,-1.,-1.3296901950568));
#22402=CARTESIAN_POINT('Ctrl Pts',(-1.61892832270724,-1.,-1.32828000610449));
#22403=CARTESIAN_POINT('Ctrl Pts',(-1.6128423401575,-1.,-1.32683074483356));
#22404=CARTESIAN_POINT('Ctrl Pts',(-1.60677758290954,-1.,-1.32534250785782));
#22405=CARTESIAN_POINT('Ctrl Pts',(-1.60073511858687,-1.,-1.32381550858256));
#22406=CARTESIAN_POINT('Ctrl Pts',(-1.59471591079403,-1.,-1.32224985747682));
#22407=CARTESIAN_POINT('Ctrl Pts',(-1.58872057258245,-1.,-1.32064537110892));
#22408=CARTESIAN_POINT('Ctrl Pts',(-1.58274907898834,-1.,-1.31900135021432));
#22409=CARTESIAN_POINT('Ctrl Pts',(-1.5768005650559,-1.,-1.31731642317187));
#22410=CARTESIAN_POINT('Ctrl Pts',(-1.57087397835723,-1.,-1.31558903860016));
#22411=CARTESIAN_POINT('Ctrl Pts',(-1.56496872402353,-1.,-1.31381795281002));
#22412=CARTESIAN_POINT('Ctrl Pts',(-1.55908521254821,-1.,-1.31200264341696));
#22413=CARTESIAN_POINT('Ctrl Pts',(-1.55322568759481,-1.,-1.31014393684222));
#22414=CARTESIAN_POINT('Ctrl Pts',(-1.54739413957185,-1.,-1.30824393907473));
#22415=CARTESIAN_POINT('Ctrl Pts',(-1.54159462645432,-1.,-1.30630475189556));
#22416=CARTESIAN_POINT('Ctrl Pts',(-1.53582981268977,-1.,-1.30432735639489));
#22417=CARTESIAN_POINT('Ctrl Pts',(-1.53009970283891,-1.,-1.30231064395568));
#22418=CARTESIAN_POINT('Ctrl Pts',(-1.52439957861062,-1.,-1.30024984366328));
#22419=CARTESIAN_POINT('Ctrl Pts',(-1.51872184912724,-1.,-1.29813791800747));
#22420=CARTESIAN_POINT('Ctrl Pts',(-1.51305994241402,-1.,-1.29596850710509));
#22421=CARTESIAN_POINT('Ctrl Pts',(-1.50741159078365,-1.,-1.29373841372842));
#22422=CARTESIAN_POINT('Ctrl Pts',(-1.50178230149776,-1.,-1.29145022885181));
#22423=CARTESIAN_POINT('Ctrl Pts',(-1.49618896881754,-1.,-1.28911506584254));
#22424=CARTESIAN_POINT('Ctrl Pts',(-1.4906522831278,-1.,-1.2867467611644));
#22425=CARTESIAN_POINT('Ctrl Pts',(-1.4851881711891,-1.,-1.28435533880201));
#22426=CARTESIAN_POINT('Ctrl Pts',(-1.47980070347095,-1.,-1.28194158939517));
#22427=CARTESIAN_POINT('Ctrl Pts',(-1.4744717526707,-1.,-1.2794891824849));
#22428=CARTESIAN_POINT('Ctrl Pts',(-1.46916035917133,-1.,-1.27696414831089));
#22429=CARTESIAN_POINT('Ctrl Pts',(-1.46382431332476,-1.,-1.27433119897822));
#22430=CARTESIAN_POINT('Ctrl Pts',(-1.45843906294697,-1.,-1.27156805265289));
#22431=CARTESIAN_POINT('Ctrl Pts',(-1.45301422764247,-1.,-1.2686778680489));
#22432=CARTESIAN_POINT('Ctrl Pts',(-1.44761985001662,-1.,-1.26570925118868));
#22433=CARTESIAN_POINT('Ctrl Pts',(-1.44236470511303,-1.,-1.26273903323859));
#22434=CARTESIAN_POINT('Ctrl Pts',(-1.43734919180848,-1.,-1.25983531012005));
#22435=CARTESIAN_POINT('Ctrl Pts',(-1.43262645609691,-1.,-1.25702687965755));
#22436=CARTESIAN_POINT('Ctrl Pts',(-1.42815938799387,-1.,-1.25426945222639));
#22437=CARTESIAN_POINT('Ctrl Pts',(-1.42378102115575,-1.,-1.2514145557001));
#22438=CARTESIAN_POINT('Ctrl Pts',(-1.41923722596025,-1.,-1.24824430986571));
#22439=CARTESIAN_POINT('Ctrl Pts',(-1.41422913175179,-1.,-1.24450600513056));
#22440=CARTESIAN_POINT('Ctrl Pts',(-1.40845295531283,-1.,-1.23994455029534));
#22441=CARTESIAN_POINT('Ctrl Pts',(-1.40164708206106,-1.,-1.23434087290423));
#22442=CARTESIAN_POINT('Ctrl Pts',(-1.39361389568796,-1.,-1.22752961899387));
#22443=CARTESIAN_POINT('Ctrl Pts',(-1.38420564527715,-1.,-1.21938737280852));
#22444=CARTESIAN_POINT('Ctrl Pts',(-1.37331915607905,-1.,-1.20982812925645));
#22445=CARTESIAN_POINT('Ctrl Pts',(-1.36088705043885,-1.,-1.1987959077932));
#22446=CARTESIAN_POINT('Ctrl Pts',(-1.34687054001093,-1.,-1.18625865667441));
#22447=CARTESIAN_POINT('Ctrl Pts',(-1.33437539347008,-1.,-1.17501305789857));
#22448=CARTESIAN_POINT('Ctrl Pts',(-1.32428080721772,-1.,-1.16589330093588));
#22449=CARTESIAN_POINT('Ctrl Pts',(-1.31722977216397,-1.,-1.15950888730809));
#22450=CARTESIAN_POINT('Ctrl Pts',(-1.31362392696032,-1.,-1.15624053661742));
#22451=CARTESIAN_POINT('',(-1.15624053661742,-1.,-1.31362392696033));
#22452=CARTESIAN_POINT('Origin',(0.,-1.,0.));
#22453=CARTESIAN_POINT('',(-1.34869019493419,-1.,-1.73811241238545));
#22454=CARTESIAN_POINT('Ctrl Pts',(-1.15624053661742,-1.,-1.31362392696033));
#22455=CARTESIAN_POINT('Ctrl Pts',(-1.15950888730433,-1.,-1.3172297721596));
#22456=CARTESIAN_POINT('Ctrl Pts',(-1.16589330092532,-1.,-1.32428080720544));
#22457=CARTESIAN_POINT('Ctrl Pts',(-1.17501305787994,-1.,-1.33437539344842));
#22458=CARTESIAN_POINT('Ctrl Pts',(-1.18625865664915,-1.,-1.34687053998157));
#22459=CARTESIAN_POINT('Ctrl Pts',(-1.1987959077656,-1.,-1.36088705040677));
#22460=CARTESIAN_POINT('Ctrl Pts',(-1.20982812923113,-1.,-1.37331915604962));
#22461=CARTESIAN_POINT('Ctrl Pts',(-1.21938737278853,-1.,-1.38420564525391));
#22462=CARTESIAN_POINT('Ctrl Pts',(-1.22752961898063,-1.,-1.39361389567257));
#22463=CARTESIAN_POINT('Ctrl Pts',(-1.23434087289768,-1.,-1.40164708205345));
#22464=CARTESIAN_POINT('Ctrl Pts',(-1.23994455029421,-1.,-1.40845295531151));
#22465=CARTESIAN_POINT('Ctrl Pts',(-1.24450600513278,-1.,-1.41422913175437));
#22466=CARTESIAN_POINT('Ctrl Pts',(-1.24824430986911,-1.,-1.41923722596421));
#22467=CARTESIAN_POINT('Ctrl Pts',(-1.25141455570299,-1.,-1.42378102115911));
#22468=CARTESIAN_POINT('Ctrl Pts',(-1.25426945222783,-1.,-1.42815938799555));
#22469=CARTESIAN_POINT('Ctrl Pts',(-1.25702687965744,-1.,-1.43262645609679));
#22470=CARTESIAN_POINT('Ctrl Pts',(-1.25983531011894,-1.,-1.43734919180719));
#22471=CARTESIAN_POINT('Ctrl Pts',(-1.26273903323723,-1.,-1.44236470511145));
#22472=CARTESIAN_POINT('Ctrl Pts',(-1.26570925118767,-1.,-1.44761985001544));
#22473=CARTESIAN_POINT('Ctrl Pts',(-1.26867786804854,-1.,-1.45301422764205));
#22474=CARTESIAN_POINT('Ctrl Pts',(-1.27156805265312,-1.,-1.45843906294725));
#22475=CARTESIAN_POINT('Ctrl Pts',(-1.27433119897877,-1.,-1.4638243133254));
#22476=CARTESIAN_POINT('Ctrl Pts',(-1.27696414831144,-1.,-1.46916035917197));
#22477=CARTESIAN_POINT('Ctrl Pts',(-1.27948918248524,-1.,-1.4744717526711));
#22478=CARTESIAN_POINT('Ctrl Pts',(-1.28194158939522,-1.,-1.47980070347102));
#22479=CARTESIAN_POINT('Ctrl Pts',(-1.28435533880184,-1.,-1.48518817118891));
#22480=CARTESIAN_POINT('Ctrl Pts',(-1.28674676116415,-1.,-1.4906522831275));
#22481=CARTESIAN_POINT('Ctrl Pts',(-1.28911506584232,-1.,-1.49618896881729));
#22482=CARTESIAN_POINT('Ctrl Pts',(-1.29145022885171,-1.,-1.50178230149764));
#22483=CARTESIAN_POINT('Ctrl Pts',(-1.29373841372843,-1.,-1.50741159078367));
#22484=CARTESIAN_POINT('Ctrl Pts',(-1.29596850710518,-1.,-1.51305994241412));
#22485=CARTESIAN_POINT('Ctrl Pts',(-1.29813791800757,-1.,-1.51872184912735));
#22486=CARTESIAN_POINT('Ctrl Pts',(-1.30024984366334,-1.,-1.5243995786107));
#22487=CARTESIAN_POINT('Ctrl Pts',(-1.3023106439557,-1.,-1.53009970283893));
#22488=CARTESIAN_POINT('Ctrl Pts',(-1.30432735639487,-1.,-1.53582981268976));
#22489=CARTESIAN_POINT('Ctrl Pts',(-1.30630475189553,-1.,-1.54159462645428));
#22490=CARTESIAN_POINT('Ctrl Pts',(-1.30824393907471,-1.,-1.54739413957183));
#22491=CARTESIAN_POINT('Ctrl Pts',(-1.31014393684221,-1.,-1.55322568759481));
#22492=CARTESIAN_POINT('Ctrl Pts',(-1.31200264341696,-1.,-1.55908521254822));
#22493=CARTESIAN_POINT('Ctrl Pts',(-1.31381795281002,-1.,-1.56496872402352));
#22494=CARTESIAN_POINT('Ctrl Pts',(-1.31558903860015,-1.,-1.57087397835721));
#22495=CARTESIAN_POINT('Ctrl Pts',(-1.31731642317183,-1.,-1.57680056505585));
#22496=CARTESIAN_POINT('Ctrl Pts',(-1.31900135021428,-1.,-1.58274907898829));
#22497=CARTESIAN_POINT('Ctrl Pts',(-1.32064537110891,-1.,-1.58872057258244));
#22498=CARTESIAN_POINT('Ctrl Pts',(-1.32224985747686,-1.,-1.59471591079408));
#22499=CARTESIAN_POINT('Ctrl Pts',(-1.32381550858266,-1.,-1.600735118587));
#22500=CARTESIAN_POINT('Ctrl Pts',(-1.32534250785794,-1.,-1.6067775829097));
#22501=CARTESIAN_POINT('Ctrl Pts',(-1.32683074483365,-1.,-1.61284234015762));
#22502=CARTESIAN_POINT('Ctrl Pts',(-1.32828000610448,-1.,-1.61892832270723));
#22503=CARTESIAN_POINT('Ctrl Pts',(-1.32969019505665,-1.,-1.62503464209777));
#22504=CARTESIAN_POINT('Ctrl Pts',(-1.33106149345618,-1.,-1.63116079730887));
#22505=CARTESIAN_POINT('Ctrl Pts',(-1.33239425103694,-1.,-1.6373065347505));
#22506=CARTESIAN_POINT('Ctrl Pts',(-1.33368890676554,-1.,-1.64347174856007));
#22507=CARTESIAN_POINT('Ctrl Pts',(-1.33494590468003,-1.,-1.64965637286843));
#22508=CARTESIAN_POINT('Ctrl Pts',(-1.33616559745217,-1.,-1.65586025952651));
#22509=CARTESIAN_POINT('Ctrl Pts',(-1.33734820885331,-1.,-1.66208312542073));
#22510=CARTESIAN_POINT('Ctrl Pts',(-1.33849388654458,-1.,-1.66832460784078));
#22511=CARTESIAN_POINT('Ctrl Pts',(-1.33960273470372,-1.,-1.67458429426126));
#22512=CARTESIAN_POINT('Ctrl Pts',(-1.3406748518516,-1.,-1.68086176030308));
#22513=CARTESIAN_POINT('Ctrl Pts',(-1.34171037484673,-1.,-1.68715660868602));
#22514=CARTESIAN_POINT('Ctrl Pts',(-1.34270948206139,-1.,-1.6934684849664));
#22515=CARTESIAN_POINT('Ctrl Pts',(-1.34367237124322,-1.,-1.69979707754221));
#22516=CARTESIAN_POINT('Ctrl Pts',(-1.34459924533783,-1.,-1.70614212266676));
#22517=CARTESIAN_POINT('Ctrl Pts',(-1.34549029589563,-1.,-1.71250340687011));
#22518=CARTESIAN_POINT('Ctrl Pts',(-1.34634568653586,-1.,-1.7188807715095));
#22519=CARTESIAN_POINT('Ctrl Pts',(-1.34716554820013,-1.,-1.72527410681298));
#22520=CARTESIAN_POINT('Ctrl Pts',(-1.3477930915247,-1.,-1.73040149654497));
#22521=CARTESIAN_POINT('Ctrl Pts',(-1.34824783113158,-1.,-1.73425417886255));
#22522=CARTESIAN_POINT('Ctrl Pts',(-1.34854391898145,-1.,-1.73682580585819));
#22523=CARTESIAN_POINT('Ctrl Pts',(-1.34869019493419,-1.,-1.73811241238545));
#22524=CARTESIAN_POINT('',(-1.23627494547115,-1.,-1.81978687191668));
#22525=CARTESIAN_POINT('',(-1.34869019493419,-1.,-1.73811241238545));
#22526=CARTESIAN_POINT('',(-0.892032620296855,-1.,-1.5055822144029));
#22527=CARTESIAN_POINT('Ctrl Pts',(-1.23627494547115,-1.,-1.81978687191668));
#22528=CARTESIAN_POINT('Ctrl Pts',(-1.23509651170384,-1.,-1.81925017193531));
#22529=CARTESIAN_POINT('Ctrl Pts',(-1.23274224526804,-1.,-1.81817389920914));
#22530=CARTESIAN_POINT('Ctrl Pts',(-1.22921864890975,-1.,-1.81655087183054));
#22531=CARTESIAN_POINT('Ctrl Pts',(-1.22453613304507,-1.,-1.81436959209778));
#22532=CARTESIAN_POINT('Ctrl Pts',(-1.2187090610323,-1.,-1.81161420806172));
#22533=CARTESIAN_POINT('Ctrl Pts',(-1.2129081570818,-1.,-1.80882996916931));
#22534=CARTESIAN_POINT('Ctrl Pts',(-1.20713356605519,-1.,-1.80601678480772));
#22535=CARTESIAN_POINT('Ctrl Pts',(-1.2013854893912,-1.,-1.8031745483882));
#22536=CARTESIAN_POINT('Ctrl Pts',(-1.19566418930405,-1.,-1.80030314370121));
#22537=CARTESIAN_POINT('Ctrl Pts',(-1.1899699793456,-1.,-1.79740245923649));
#22538=CARTESIAN_POINT('Ctrl Pts',(-1.18430321697471,-1.,-1.79447240321572));
#22539=CARTESIAN_POINT('Ctrl Pts',(-1.17866429440781,-1.,-1.79151291552646));
#22540=CARTESIAN_POINT('Ctrl Pts',(-1.17305363177265,-1.,-1.78852398877523));
#22541=CARTESIAN_POINT('Ctrl Pts',(-1.16747166312239,-1.,-1.78550566040349));
#22542=CARTESIAN_POINT('Ctrl Pts',(-1.16191881298458,-1.,-1.78245795880949));
#22543=CARTESIAN_POINT('Ctrl Pts',(-1.15639547194689,-1.,-1.77938085564261));
#22544=CARTESIAN_POINT('Ctrl Pts',(-1.15090197841531,-1.,-1.77627422557034));
#22545=CARTESIAN_POINT('Ctrl Pts',(-1.14543858226948,-1.,-1.77313777896234));
#22546=CARTESIAN_POINT('Ctrl Pts',(-1.14000548337,-1.,-1.76997111386806));
#22547=CARTESIAN_POINT('Ctrl Pts',(-1.13460291804635,-1.,-1.76677384551883));
#22548=CARTESIAN_POINT('Ctrl Pts',(-1.12923123555076,-1.,-1.76354571966171));
#22549=CARTESIAN_POINT('Ctrl Pts',(-1.12389096855078,-1.,-1.76028671825084));
#22550=CARTESIAN_POINT('Ctrl Pts',(-1.11858293216752,-1.,-1.75699720772089));
#22551=CARTESIAN_POINT('Ctrl Pts',(-1.11330807582542,-1.,-1.75367772094617));
#22552=CARTESIAN_POINT('Ctrl Pts',(-1.10806728183003,-1.,-1.75032866075914));
#22553=CARTESIAN_POINT('Ctrl Pts',(-1.10286118991144,-1.,-1.74695004214924));
#22554=CARTESIAN_POINT('Ctrl Pts',(-1.09768999241229,-1.,-1.74354119236212));
#22555=CARTESIAN_POINT('Ctrl Pts',(-1.09255329056496,-1.,-1.74010053962252));
#22556=CARTESIAN_POINT('Ctrl Pts',(-1.08745056285429,-1.,-1.73662628326093));
#22557=CARTESIAN_POINT('Ctrl Pts',(-1.08238162784749,-1.,-1.73311705663407));
#22558=CARTESIAN_POINT('Ctrl Pts',(-1.0773470373727,-1.,-1.72957248977424));
#22559=CARTESIAN_POINT('Ctrl Pts',(-1.07234866990252,-1.,-1.72599406198489));
#22560=CARTESIAN_POINT('Ctrl Pts',(-1.06738966975463,-1.,-1.72238500928456));
#22561=CARTESIAN_POINT('Ctrl Pts',(-1.0624732468065,-1.,-1.71874858456908));
#22562=CARTESIAN_POINT('Ctrl Pts',(-1.05760163192481,-1.,-1.71508654427022));
#22563=CARTESIAN_POINT('Ctrl Pts',(-1.05277517202854,-1.,-1.71139783543986));
#22564=CARTESIAN_POINT('Ctrl Pts',(-1.0479908540499,-1.,-1.70767646263641));
#22565=CARTESIAN_POINT('Ctrl Pts',(-1.04324363334546,-1.,-1.70391338707969));
#22566=CARTESIAN_POINT('Ctrl Pts',(-1.03852922490782,-1.,-1.70010052930951));
#22567=CARTESIAN_POINT('Ctrl Pts',(-1.03384646003587,-1.,-1.69623414782769));
#22568=CARTESIAN_POINT('Ctrl Pts',(-1.02919977579155,-1.,-1.69231840863471));
#22569=CARTESIAN_POINT('Ctrl Pts',(-1.02460180535272,-1.,-1.68836910178475));
#22570=CARTESIAN_POINT('Ctrl Pts',(-1.02006795074222,-1.,-1.68440578021739));
#22571=CARTESIAN_POINT('Ctrl Pts',(-1.01561026162787,-1.,-1.6804428989482));
#22572=CARTESIAN_POINT('Ctrl Pts',(-1.01123236493507,-1.,-1.67648246776457));
#22573=CARTESIAN_POINT('Ctrl Pts',(-1.00692206696387,-1.,-1.67250335383248));
#22574=CARTESIAN_POINT('Ctrl Pts',(-1.00265091003682,-1.,-1.66846059277231));
#22575=CARTESIAN_POINT('Ctrl Pts',(-0.998389654952317,-1.,-1.66430758030304));
#22576=CARTESIAN_POINT('Ctrl Pts',(-0.994121836661116,-1.,-1.66001553809916));
#22577=CARTESIAN_POINT('Ctrl Pts',(-0.98985562785445,-1.,-1.65559044289746));
#22578=CARTESIAN_POINT('Ctrl Pts',(-0.985642622921626,-1.,-1.6511001661277));
#22579=CARTESIAN_POINT('Ctrl Pts',(-0.981562530940574,-1.,-1.64665139190834));
#22580=CARTESIAN_POINT('Ctrl Pts',(-0.977689794120297,-1.,-1.64233990826831));
#22581=CARTESIAN_POINT('Ctrl Pts',(-0.974066058287501,-1.,-1.63820952658157));
#22582=CARTESIAN_POINT('Ctrl Pts',(-0.970669715996356,-1.,-1.63420665729609));
#22583=CARTESIAN_POINT('Ctrl Pts',(-0.967387853228041,-1.,-1.63013849959083));
#22584=CARTESIAN_POINT('Ctrl Pts',(-0.964046107037821,-1.,-1.6257193066974));
#22585=CARTESIAN_POINT('Ctrl Pts',(-0.960438326099958,-1.,-1.62061638139929));
#22586=CARTESIAN_POINT('Ctrl Pts',(-0.956354422921573,-1.,-1.61449324337233));
#22587=CARTESIAN_POINT('Ctrl Pts',(-0.951613284361248,-1.,-1.60706069897794));
#22588=CARTESIAN_POINT('Ctrl Pts',(-0.946078063325796,-1.,-1.59810042045408));
#22589=CARTESIAN_POINT('Ctrl Pts',(-0.939646377909319,-1.,-1.58744937489796));
#22590=CARTESIAN_POINT('Ctrl Pts',(-0.932246680128849,-1.,-1.57499388385561));
#22591=CARTESIAN_POINT('Ctrl Pts',(-0.923832188966322,-1.,-1.56065988582509));
#22592=CARTESIAN_POINT('Ctrl Pts',(-0.91437591904658,-1.,-1.54440491152808));
#22593=CARTESIAN_POINT('Ctrl Pts',(-0.905967409640499,-1.,-1.52984849890434));
#22594=CARTESIAN_POINT('Ctrl Pts',(-0.89918504749193,-1.,-1.51805569591479));
#22595=CARTESIAN_POINT('Ctrl Pts',(-0.894452006967538,-1.,-1.50980486807181));
#22596=CARTESIAN_POINT('Ctrl Pts',(-0.892032620296855,-1.,-1.5055822144029));
#22597=CARTESIAN_POINT('',(-0.693717979106305,-1.,-1.60662857109684));
#22598=CARTESIAN_POINT('Origin',(0.,-1.,0.));
#22599=CARTESIAN_POINT('',(-0.745574324794401,-1.,-2.0698113262342));
#22600=CARTESIAN_POINT('Ctrl Pts',(-0.693717979106305,-1.,-1.60662857109684));
#22601=CARTESIAN_POINT('Ctrl Pts',(-0.69571209787897,-1.,-1.61106790957619));
#22602=CARTESIAN_POINT('Ctrl Pts',(-0.699605146398837,-1.,-1.61974673471117));
#22603=CARTESIAN_POINT('Ctrl Pts',(-0.705159151977294,-1.,-1.6321654166204));
#22604=CARTESIAN_POINT('Ctrl Pts',(-0.711993139340447,-1.,-1.64752408828442));
#22605=CARTESIAN_POINT('Ctrl Pts',(-0.71958543378795,-1.,-1.66472880551777));
#22606=CARTESIAN_POINT('Ctrl Pts',(-0.726235967982445,-1.,-1.67996158451922));
#22607=CARTESIAN_POINT('Ctrl Pts',(-0.731963238685357,-1.,-1.69326921972915));
#22608=CARTESIAN_POINT('Ctrl Pts',(-0.736799665716932,-1.,-1.70473309004249));
#22609=CARTESIAN_POINT('Ctrl Pts',(-0.74079516202821,-1.,-1.71447789751001));
#22610=CARTESIAN_POINT('Ctrl Pts',(-0.744021445433093,-1.,-1.72268229916769));
#22611=CARTESIAN_POINT('Ctrl Pts',(-0.746574710097752,-1.,-1.72958533647714));
#22612=CARTESIAN_POINT('Ctrl Pts',(-0.74858246295687,-1.,-1.7355035168033));
#22613=CARTESIAN_POINT('Ctrl Pts',(-0.750193435981249,-1.,-1.74080458267114));
#22614=CARTESIAN_POINT('Ctrl Pts',(-0.751555614164482,-1.,-1.74585086852502));
#22615=CARTESIAN_POINT('Ctrl Pts',(-0.752797683531314,-1.,-1.75095139468794));
#22616=CARTESIAN_POINT('Ctrl Pts',(-0.754009254027829,-1.,-1.75631083600019));
#22617=CARTESIAN_POINT('Ctrl Pts',(-0.755220979974461,-1.,-1.76197817240128));
#22618=CARTESIAN_POINT('Ctrl Pts',(-0.75642189602781,-1.,-1.76789396002998));
#22619=CARTESIAN_POINT('Ctrl Pts',(-0.757578264077029,-1.,-1.77394167108292));
#22620=CARTESIAN_POINT('Ctrl Pts',(-0.758650626677518,-1.,-1.77999411220945));
#22621=CARTESIAN_POINT('Ctrl Pts',(-0.759614401110189,-1.,-1.78596964884604));
#22622=CARTESIAN_POINT('Ctrl Pts',(-0.760469555880749,-1.,-1.7918581561088));
#22623=CARTESIAN_POINT('Ctrl Pts',(-0.761229695230558,-1.,-1.79768986997783));
#22624=CARTESIAN_POINT('Ctrl Pts',(-0.761915336443547,-1.,-1.80351583877342));
#22625=CARTESIAN_POINT('Ctrl Pts',(-0.762546129463938,-1.,-1.80938551463965));
#22626=CARTESIAN_POINT('Ctrl Pts',(-0.763132003836634,-1.,-1.8153211840553));
#22627=CARTESIAN_POINT('Ctrl Pts',(-0.763673465462726,-1.,-1.82131873145266));
#22628=CARTESIAN_POINT('Ctrl Pts',(-0.764165902605995,-1.,-1.82735991200065));
#22629=CARTESIAN_POINT('Ctrl Pts',(-0.764602549687853,-1.,-1.83342077227142));
#22630=CARTESIAN_POINT('Ctrl Pts',(-0.764978057881737,-1.,-1.83948181064835));
#22631=CARTESIAN_POINT('Ctrl Pts',(-0.765291664862029,-1.,-1.84553698875924));
#22632=CARTESIAN_POINT('Ctrl Pts',(-0.765545710619062,-1.,-1.85158945130063));
#22633=CARTESIAN_POINT('Ctrl Pts',(-0.765744212909318,-1.,-1.85764741390394));
#22634=CARTESIAN_POINT('Ctrl Pts',(-0.765891519092547,-1.,-1.86372027063312));
#22635=CARTESIAN_POINT('Ctrl Pts',(-0.765990708546091,-1.,-1.86981398314341));
#22636=CARTESIAN_POINT('Ctrl Pts',(-0.766042837036744,-1.,-1.87592888967883));
#22637=CARTESIAN_POINT('Ctrl Pts',(-0.766047794851865,-1.,-1.88206215302561));
#22638=CARTESIAN_POINT('Ctrl Pts',(-0.766004837062091,-1.,-1.88820926433409));
#22639=CARTESIAN_POINT('Ctrl Pts',(-0.765913193856978,-1.,-1.89436577771388));
#22640=CARTESIAN_POINT('Ctrl Pts',(-0.765772772593386,-1.,-1.90052930393596));
#22641=CARTESIAN_POINT('Ctrl Pts',(-0.765584196937919,-1.,-1.90669961402356));
#22642=CARTESIAN_POINT('Ctrl Pts',(-0.765348465884722,-1.,-1.91287765805169));
#22643=CARTESIAN_POINT('Ctrl Pts',(-0.765066729667088,-1.,-1.91906491634196));
#22644=CARTESIAN_POINT('Ctrl Pts',(-0.764740025488211,-1.,-1.92526263537048));
#22645=CARTESIAN_POINT('Ctrl Pts',(-0.764369010673941,-1.,-1.93147105496382));
#22646=CARTESIAN_POINT('Ctrl Pts',(-0.763954049121458,-1.,-1.93768964875886));
#22647=CARTESIAN_POINT('Ctrl Pts',(-0.763495333538629,-1.,-1.9439174661764));
#22648=CARTESIAN_POINT('Ctrl Pts',(-0.762992990878769,-1.,-1.95015342590024));
#22649=CARTESIAN_POINT('Ctrl Pts',(-0.762447203806179,-1.,-1.95639665309869));
#22650=CARTESIAN_POINT('Ctrl Pts',(-0.761858300014423,-1.,-1.96264672744186));
#22651=CARTESIAN_POINT('Ctrl Pts',(-0.76122669048382,-1.,-1.96890351582499));
#22652=CARTESIAN_POINT('Ctrl Pts',(-0.760552825409757,-1.,-1.97516705321494));
#22653=CARTESIAN_POINT('Ctrl Pts',(-0.75983714745219,-1.,-1.98143741418172));
#22654=CARTESIAN_POINT('Ctrl Pts',(-0.759080037802488,-1.,-1.98771456680874));
#22655=CARTESIAN_POINT('Ctrl Pts',(-0.758281796766761,-1.,-1.99399831098817));
#22656=CARTESIAN_POINT('Ctrl Pts',(-0.757442676862724,-1.,-2.00028834739178));
#22657=CARTESIAN_POINT('Ctrl Pts',(-0.75656290464667,-1.,-2.0065843158773));
#22658=CARTESIAN_POINT('Ctrl Pts',(-0.755642704957865,-1.,-2.01288584328084));
#22659=CARTESIAN_POINT('Ctrl Pts',(-0.754682330722816,-1.,-2.01919259405809));
#22660=CARTESIAN_POINT('Ctrl Pts',(-0.753682061112768,-1.,-2.02550428623313));
#22661=CARTESIAN_POINT('Ctrl Pts',(-0.752642180487211,-1.,-2.03182068456221));
#22662=CARTESIAN_POINT('Ctrl Pts',(-0.751562963361115,-1.,-2.03814160092099));
#22663=CARTESIAN_POINT('Ctrl Pts',(-0.750444657875576,-1.,-2.04446689147979));
#22664=CARTESIAN_POINT('Ctrl Pts',(-0.749287468665046,-1.,-2.05079645592154));
#22665=CARTESIAN_POINT('Ctrl Pts',(-0.748091554183802,-1.,-2.05713023031006));
#22666=CARTESIAN_POINT('Ctrl Pts',(-0.747103932787919,-1.,-2.06220058927826));
#22667=CARTESIAN_POINT('Ctrl Pts',(-0.7463458715442,-1.,-2.06600523016815));
#22668=CARTESIAN_POINT('Ctrl Pts',(-0.745832791378367,-1.,-2.06854248895728));
#22669=CARTESIAN_POINT('Ctrl Pts',(-0.745574324794401,-1.,-2.0698113262342));
#22670=CARTESIAN_POINT('',(-0.61342227326009,-1.,-2.11275013067528));
#22671=CARTESIAN_POINT('',(-0.745574324794401,-1.,-2.0698113262342));
#22672=CARTESIAN_POINT('',(-0.383122945602004,-1.,-1.7075470150345));
#22673=CARTESIAN_POINT('Ctrl Pts',(-0.61342227326009,-1.,-2.11275013067528));
#22674=CARTESIAN_POINT('Ctrl Pts',(-0.6124673655618,-1.,-2.11187554259986));
#22675=CARTESIAN_POINT('Ctrl Pts',(-0.610560911689899,-1.,-2.11012443807238));
#22676=CARTESIAN_POINT('Ctrl Pts',(-0.607711315454876,-1.,-2.1074919961518));
#22677=CARTESIAN_POINT('Ctrl Pts',(-0.60393203073603,-1.,-2.10397049886949));
#22678=CARTESIAN_POINT('Ctrl Pts',(-0.599241616420533,-1.,-2.0995493086477));
#22679=CARTESIAN_POINT('Ctrl Pts',(-0.594585006052162,-1.,-2.0951087622027));
#22680=CARTESIAN_POINT('Ctrl Pts',(-0.589962365403406,-1.,-2.09064881812129));
#22681=CARTESIAN_POINT('Ctrl Pts',(-0.585373918991617,-1.,-2.08616943727951));
#22682=CARTESIAN_POINT('Ctrl Pts',(-0.580819952108063,-1.,-2.08167059018418));
#22683=CARTESIAN_POINT('Ctrl Pts',(-0.576300797416844,-1.,-2.07715226767559));
#22684=CARTESIAN_POINT('Ctrl Pts',(-0.571816823242603,-1.,-2.07261449292824));
#22685=CARTESIAN_POINT('Ctrl Pts',(-0.567368421181087,-1.,-2.06805732997334));
#22686=CARTESIAN_POINT('Ctrl Pts',(-0.562955993082261,-1.,-2.06348090160589));
#22687=CARTESIAN_POINT('Ctrl Pts',(-0.558579940185151,-1.,-2.05888537756462));
#22688=CARTESIAN_POINT('Ctrl Pts',(-0.554240657463906,-1.,-2.05427091604413));
#22689=CARTESIAN_POINT('Ctrl Pts',(-0.549938525150295,-1.,-2.04963761077958));
#22690=CARTESIAN_POINT('Ctrl Pts',(-0.54567390381743,-1.,-2.04498544714588));
#22691=CARTESIAN_POINT('Ctrl Pts',(-0.541447120615659,-1.,-2.04031422690527));
#22692=CARTESIAN_POINT('Ctrl Pts',(-0.537258489833262,-1.,-2.03562362954037));
#22693=CARTESIAN_POINT('Ctrl Pts',(-0.533108355132977,-1.,-2.03091336214426));
#22694=CARTESIAN_POINT('Ctrl Pts',(-0.528997127241914,-1.,-2.0261832908329));
#22695=CARTESIAN_POINT('Ctrl Pts',(-0.524925318333476,-1.,-2.02143356304698));
#22696=CARTESIAN_POINT('Ctrl Pts',(-0.52089359039937,-1.,-2.01666477917286));
#22697=CARTESIAN_POINT('Ctrl Pts',(-0.516902681728687,-1.,-2.01187773939242));
#22698=CARTESIAN_POINT('Ctrl Pts',(-0.512953306961792,-1.,-2.00707309946949));
#22699=CARTESIAN_POINT('Ctrl Pts',(-0.509046069886157,-1.,-2.00225107134734));
#22700=CARTESIAN_POINT('Ctrl Pts',(-0.505181361323026,-1.,-1.99741107463572));
#22701=CARTESIAN_POINT('Ctrl Pts',(-0.501359287727146,-1.,-1.99255149126155));
#22702=CARTESIAN_POINT('Ctrl Pts',(-0.497579909545574,-1.,-1.98767044752932));
#22703=CARTESIAN_POINT('Ctrl Pts',(-0.493843476541495,-1.,-1.98276658761821));
#22704=CARTESIAN_POINT('Ctrl Pts',(-0.490150627860952,-1.,-1.97783973019229));
#22705=CARTESIAN_POINT('Ctrl Pts',(-0.486502692907659,-1.,-1.97289186263272));
#22706=CARTESIAN_POINT('Ctrl Pts',(-0.482901662120691,-1.,-1.96792703422362));
#22707=CARTESIAN_POINT('Ctrl Pts',(-0.479349583074855,-1.,-1.96294933055943));
#22708=CARTESIAN_POINT('Ctrl Pts',(-0.475848034683176,-1.,-1.95796111148177));
#22709=CARTESIAN_POINT('Ctrl Pts',(-0.472397672264072,-1.,-1.95296148278133));
#22710=CARTESIAN_POINT('Ctrl Pts',(-0.468997482913135,-1.,-1.94794381136514));
#22711=CARTESIAN_POINT('Ctrl Pts',(-0.46564546202603,-1.,-1.9428979419619));
#22712=CARTESIAN_POINT('Ctrl Pts',(-0.462340031009056,-1.,-1.93781486640821));
#22713=CARTESIAN_POINT('Ctrl Pts',(-0.459081234547926,-1.,-1.93269066517934));
#22714=CARTESIAN_POINT('Ctrl Pts',(-0.455872005174371,-1.,-1.92753067150476));
#22715=CARTESIAN_POINT('Ctrl Pts',(-0.452719478359432,-1.,-1.92235380648502));
#22716=CARTESIAN_POINT('Ctrl Pts',(-0.449632260106662,-1.,-1.91718342555755));
#22717=CARTESIAN_POINT('Ctrl Pts',(-0.446617343485711,-1.,-1.9120369998112));
#22718=CARTESIAN_POINT('Ctrl Pts',(-0.443677556849151,-1.,-1.90691756144898));
#22719=CARTESIAN_POINT('Ctrl Pts',(-0.440807833704038,-1.,-1.90180124389086));
#22720=CARTESIAN_POINT('Ctrl Pts',(-0.437995003948244,-1.,-1.89663648956466));
#22721=CARTESIAN_POINT('Ctrl Pts',(-0.435225660963383,-1.,-1.89136993975504));
#22722=CARTESIAN_POINT('Ctrl Pts',(-0.432493038548748,-1.,-1.88596913666793));
#22723=CARTESIAN_POINT('Ctrl Pts',(-0.429803062482344,-1.,-1.88044229001832));
#22724=CARTESIAN_POINT('Ctrl Pts',(-0.427183828519102,-1.,-1.87486989291484));
#22725=CARTESIAN_POINT('Ctrl Pts',(-0.424678177291359,-1.,-1.86937803944323));
#22726=CARTESIAN_POINT('Ctrl Pts',(-0.422327307418275,-1.,-1.86408083334028));
#22727=CARTESIAN_POINT('Ctrl Pts',(-0.420157287975619,-1.,-1.85903281096686));
#22728=CARTESIAN_POINT('Ctrl Pts',(-0.418164129143534,-1.,-1.85417632856234));
#22729=CARTESIAN_POINT('Ctrl Pts',(-0.416300022038864,-1.,-1.84929312929882));
#22730=CARTESIAN_POINT('Ctrl Pts',(-0.41448743825434,-1.,-1.8440575707371));
#22731=CARTESIAN_POINT('Ctrl Pts',(-0.412633125322162,-1.,-1.83808953475839));
#22732=CARTESIAN_POINT('Ctrl Pts',(-0.410641256301675,-1.,-1.83100408895216));
#22733=CARTESIAN_POINT('Ctrl Pts',(-0.408428948108533,-1.,-1.8224702267854));
#22734=CARTESIAN_POINT('Ctrl Pts',(-0.405933518411838,-1.,-1.81223801813988));
#22735=CARTESIAN_POINT('Ctrl Pts',(-0.403107976170441,-1.,-1.80012077176221));
#22736=CARTESIAN_POINT('Ctrl Pts',(-0.39991940378308,-1.,-1.78598826347533));
#22737=CARTESIAN_POINT('Ctrl Pts',(-0.39634619612042,-1.,-1.7697556004756));
#22738=CARTESIAN_POINT('Ctrl Pts',(-0.392375812294307,-1.,-1.75137405313962));
#22739=CARTESIAN_POINT('Ctrl Pts',(-0.388877023509191,-1.,-1.7349317097561));
#22740=CARTESIAN_POINT('Ctrl Pts',(-0.38607079032701,-1.,-1.72162022246158));
#22741=CARTESIAN_POINT('Ctrl Pts',(-0.384119047315542,-1.,-1.71231062891958));
#22742=CARTESIAN_POINT('Ctrl Pts',(-0.383122945602004,-1.,-1.7075470150345));
#22743=CARTESIAN_POINT('',(-0.163289472382896,-1.,-1.74236521665491));
#22744=CARTESIAN_POINT('Origin',(0.,-1.,0.));
#22745=CARTESIAN_POINT('',(-0.0694764450219581,-1.,-2.19890268624765));
#22746=CARTESIAN_POINT('Ctrl Pts',(-0.163289472382896,-1.,-1.74236521665491));
#22747=CARTESIAN_POINT('Ctrl Pts',(-0.163814161002002,-1.,-1.7472034950333));
#22748=CARTESIAN_POINT('Ctrl Pts',(-0.164834765707158,-1.,-1.75666056638427));
#22749=CARTESIAN_POINT('Ctrl Pts',(-0.1662793551464,-1.,-1.77018771684844));
#22750=CARTESIAN_POINT('Ctrl Pts',(-0.168032772805197,-1.,-1.7869064998507));
#22751=CARTESIAN_POINT('Ctrl Pts',(-0.169936923904608,-1.,-1.80561530629706));
#22752=CARTESIAN_POINT('Ctrl Pts',(-0.171554770204119,-1.,-1.82215766811545));
#22753=CARTESIAN_POINT('Ctrl Pts',(-0.1728894428919,-1.,-1.83658380527692));
#22754=CARTESIAN_POINT('Ctrl Pts',(-0.173946627587731,-1.,-1.8489811319852));
#22755=CARTESIAN_POINT('Ctrl Pts',(-0.17473525927603,-1.,-1.85948367088837));
#22756=CARTESIAN_POINT('Ctrl Pts',(-0.175268337590758,-1.,-1.86828349694799));
#22757=CARTESIAN_POINT('Ctrl Pts',(-0.175563480746485,-1.,-1.87563767773588));
#22758=CARTESIAN_POINT('Ctrl Pts',(-0.175644148889699,-1.,-1.88188663145367));
#22759=CARTESIAN_POINT('Ctrl Pts',(-0.175538155840648,-1.,-1.88742606273259));
#22760=CARTESIAN_POINT('Ctrl Pts',(-0.175274276190844,-1.,-1.892646301985));
#22761=CARTESIAN_POINT('Ctrl Pts',(-0.174879405091263,-1.,-1.89788101117132));
#22762=CARTESIAN_POINT('Ctrl Pts',(-0.174375518661085,-1.,-1.90335253862834));
#22763=CARTESIAN_POINT('Ctrl Pts',(-0.173776635257817,-1.,-1.90911693975267));
#22764=CARTESIAN_POINT('Ctrl Pts',(-0.173090695383496,-1.,-1.91511429159527));
#22765=CARTESIAN_POINT('Ctrl Pts',(-0.172321621259514,-1.,-1.9212233439798));
#22766=CARTESIAN_POINT('Ctrl Pts',(-0.171471191532988,-1.,-1.92731093582036));
#22767=CARTESIAN_POINT('Ctrl Pts',(-0.170541253116202,-1.,-1.93329183155539));
#22768=CARTESIAN_POINT('Ctrl Pts',(-0.169534904817491,-1.,-1.93915639211581));
#22769=CARTESIAN_POINT('Ctrl Pts',(-0.168455741607556,-1.,-1.94493757756931));
#22770=CARTESIAN_POINT('Ctrl Pts',(-0.167307501784475,-1.,-1.95069027794294));
#22771=CARTESIAN_POINT('Ctrl Pts',(-0.166093592002812,-1.,-1.9564675971873));
#22772=CARTESIAN_POINT('Ctrl Pts',(-0.164816568920269,-1.,-1.96229379940136));
#22773=CARTESIAN_POINT('Ctrl Pts',(-0.163478185457734,-1.,-1.96816512677967));
#22774=CARTESIAN_POINT('Ctrl Pts',(-0.162079693556289,-1.,-1.97406280235188));
#22775=CARTESIAN_POINT('Ctrl Pts',(-0.160622060784611,-1.,-1.97996195437559));
#22776=CARTESIAN_POINT('Ctrl Pts',(-0.159106226437299,-1.,-1.98584238283292));
#22777=CARTESIAN_POINT('Ctrl Pts',(-0.157533331459227,-1.,-1.99169810931908));
#22778=CARTESIAN_POINT('Ctrl Pts',(-0.155904629548783,-1.,-1.99753284771497));
#22779=CARTESIAN_POINT('Ctrl Pts',(-0.154221403049722,-1.,-2.00335565310543));
#22780=CARTESIAN_POINT('Ctrl Pts',(-0.15248488362145,-1.,-2.00917680318424));
#22781=CARTESIAN_POINT('Ctrl Pts',(-0.150696157673078,-1.,-2.01500291940238));
#22782=CARTESIAN_POINT('Ctrl Pts',(-0.148856124775337,-1.,-2.02083464969894));
#22783=CARTESIAN_POINT('Ctrl Pts',(-0.146965557332583,-1.,-2.02666926182017));
#22784=CARTESIAN_POINT('Ctrl Pts',(-0.145025140186057,-1.,-2.03250223739942));
#22785=CARTESIAN_POINT('Ctrl Pts',(-0.143035515058209,-1.,-2.03832911025912));
#22786=CARTESIAN_POINT('Ctrl Pts',(-0.140997332152546,-1.,-2.04414757947916));
#22787=CARTESIAN_POINT('Ctrl Pts',(-0.138911255368966,-1.,-2.04995762001328));
#22788=CARTESIAN_POINT('Ctrl Pts',(-0.136777941218044,-1.,-2.05576044414264));
#22789=CARTESIAN_POINT('Ctrl Pts',(-0.134598026192106,-1.,-2.06155781517842));
#22790=CARTESIAN_POINT('Ctrl Pts',(-0.13237211154771,-1.,-2.06735123910326));
#22791=CARTESIAN_POINT('Ctrl Pts',(-0.130100748328403,-1.,-2.07314114713063));
#22792=CARTESIAN_POINT('Ctrl Pts',(-0.12778444527612,-1.,-2.07892715110987));
#22793=CARTESIAN_POINT('Ctrl Pts',(-0.125423679412061,-1.,-2.08470840653643));
#22794=CARTESIAN_POINT('Ctrl Pts',(-0.123018905621083,-1.,-2.09048392424825));
#22795=CARTESIAN_POINT('Ctrl Pts',(-0.120570567965122,-1.,-2.0962529286773));
#22796=CARTESIAN_POINT('Ctrl Pts',(-0.118079107988355,-1.,-2.102015121329));
#22797=CARTESIAN_POINT('Ctrl Pts',(-0.115544957687926,-1.,-2.10777050261309));
#22798=CARTESIAN_POINT('Ctrl Pts',(-0.112968534419737,-1.,-2.11351924490306));
#22799=CARTESIAN_POINT('Ctrl Pts',(-0.110350236135025,-1.,-2.11926155590865));
#22800=CARTESIAN_POINT('Ctrl Pts',(-0.10769043523109,-1.,-2.12499752307));
#22801=CARTESIAN_POINT('Ctrl Pts',(-0.104989479152739,-1.,-2.13072704887293));
#22802=CARTESIAN_POINT('Ctrl Pts',(-0.1022477005561,-1.,-2.13644992667165));
#22803=CARTESIAN_POINT('Ctrl Pts',(-0.0994654261990915,-1.,-2.14216588396025));
#22804=CARTESIAN_POINT('Ctrl Pts',(-0.0966429852305459,-1.,-2.14787463531795));
#22805=CARTESIAN_POINT('Ctrl Pts',(-0.0937807218867643,-1.,-2.1535759397817));
#22806=CARTESIAN_POINT('Ctrl Pts',(-0.0908789888107265,-1.,-2.15926961544516));
#22807=CARTESIAN_POINT('Ctrl Pts',(-0.0879381291386923,-1.,-2.16495552645014));
#22808=CARTESIAN_POINT('Ctrl Pts',(-0.0849584620835372,-1.,-2.17063357870952));
#22809=CARTESIAN_POINT('Ctrl Pts',(-0.0819402680872765,-1.,-2.176303712113));
#22810=CARTESIAN_POINT('Ctrl Pts',(-0.0788837727685243,-1.,-2.18196589448887));
#22811=CARTESIAN_POINT('Ctrl Pts',(-0.0757891465836148,-1.,-2.1876201139953));
#22812=CARTESIAN_POINT('Ctrl Pts',(-0.0732830357306725,-1.,-2.19213712013662));
#22813=CARTESIAN_POINT('Ctrl Pts',(-0.0713863779526154,-1.,-2.19552129484002));
#22814=CARTESIAN_POINT('Ctrl Pts',(-0.070114353632549,-1.,-2.19777582085423));
#22815=CARTESIAN_POINT('Ctrl Pts',(-0.0694764450219581,-1.,-2.19890268624765));
#22816=CARTESIAN_POINT('',(0.0694764450219584,-1.,-2.19890268624765));
#22817=CARTESIAN_POINT('',(-0.0694764450219581,-1.,-2.19890268624765));
#22818=CARTESIAN_POINT('',(0.163289472382896,-1.,-1.74236521665491));
#22819=CARTESIAN_POINT('Ctrl Pts',(0.0694764450219584,-1.,-2.19890268624765));
#22820=CARTESIAN_POINT('Ctrl Pts',(0.0701143536324926,-1.,-2.19777582085261));
#22821=CARTESIAN_POINT('Ctrl Pts',(0.0713863779524627,-1.,-2.19552129483562));
#22822=CARTESIAN_POINT('Ctrl Pts',(0.0732830357304276,-1.,-2.19213712012956));
#22823=CARTESIAN_POINT('Ctrl Pts',(0.0757891465833411,-1.,-2.1876201139874));
#22824=CARTESIAN_POINT('Ctrl Pts',(0.0788837727683228,-1.,-2.18196589448304));
#22825=CARTESIAN_POINT('Ctrl Pts',(0.0819402680871939,-1.,-2.1763037121106));
#22826=CARTESIAN_POINT('Ctrl Pts',(0.0849584620835643,-1.,-2.17063357871031));
#22827=CARTESIAN_POINT('Ctrl Pts',(0.0879381291387823,-1.,-2.16495552645275));
#22828=CARTESIAN_POINT('Ctrl Pts',(0.0908789888108266,-1.,-2.15926961544808));
#22829=CARTESIAN_POINT('Ctrl Pts',(0.0937807218868345,-1.,-2.15357593978377));
#22830=CARTESIAN_POINT('Ctrl Pts',(0.0966429852305689,-1.,-2.14787463531864));
#22831=CARTESIAN_POINT('Ctrl Pts',(0.0994654261990743,-1.,-2.14216588395974));
#22832=CARTESIAN_POINT('Ctrl Pts',(0.102247700556064,-1.,-2.13644992667052));
#22833=CARTESIAN_POINT('Ctrl Pts',(0.104989479152703,-1.,-2.1307270488718));
#22834=CARTESIAN_POINT('Ctrl Pts',(0.107690435231068,-1.,-2.12499752306927));
#22835=CARTESIAN_POINT('Ctrl Pts',(0.11035023613502,-1.,-2.11926155590849));
#22836=CARTESIAN_POINT('Ctrl Pts',(0.112968534419746,-1.,-2.11351924490335));
#22837=CARTESIAN_POINT('Ctrl Pts',(0.11554495768794,-1.,-2.10777050261359));
#22838=CARTESIAN_POINT('Ctrl Pts',(0.118079107988368,-1.,-2.10201512132945));
#22839=CARTESIAN_POINT('Ctrl Pts',(0.120570567965129,-1.,-2.09625292867756));
#22840=CARTESIAN_POINT('Ctrl Pts',(0.123018905621083,-1.,-2.09048392424826));
#22841=CARTESIAN_POINT('Ctrl Pts',(0.125423679412058,-1.,-2.08470840653628));
#22842=CARTESIAN_POINT('Ctrl Pts',(0.127784445276116,-1.,-2.07892715110967));
#22843=CARTESIAN_POINT('Ctrl Pts',(0.1301007483284,-1.,-2.07314114713047));
#22844=CARTESIAN_POINT('Ctrl Pts',(0.13237211154771,-1.,-2.06735123910319));
#22845=CARTESIAN_POINT('Ctrl Pts',(0.134598026192107,-1.,-2.06155781517844));
#22846=CARTESIAN_POINT('Ctrl Pts',(0.136777941218044,-1.,-2.0557604441427));
#22847=CARTESIAN_POINT('Ctrl Pts',(0.138911255368966,-1.,-2.04995762001333));
#22848=CARTESIAN_POINT('Ctrl Pts',(0.140997332152545,-1.,-2.04414757947919));
#22849=CARTESIAN_POINT('Ctrl Pts',(0.143035515058208,-1.,-2.03832911025913));
#22850=CARTESIAN_POINT('Ctrl Pts',(0.145025140186058,-1.,-2.03250223739941));
#22851=CARTESIAN_POINT('Ctrl Pts',(0.146965557332586,-1.,-2.02666926182017));
#22852=CARTESIAN_POINT('Ctrl Pts',(0.148856124775343,-1.,-2.02083464969897));
#22853=CARTESIAN_POINT('Ctrl Pts',(0.150696157673084,-1.,-2.01500291940243));
#22854=CARTESIAN_POINT('Ctrl Pts',(0.152484883621452,-1.,-2.00917680318426));
#22855=CARTESIAN_POINT('Ctrl Pts',(0.154221403049719,-1.,-2.00335565310539));
#22856=CARTESIAN_POINT('Ctrl Pts',(0.155904629548774,-1.,-1.99753284771487));
#22857=CARTESIAN_POINT('Ctrl Pts',(0.157533331459215,-1.,-1.99169810931893));
#22858=CARTESIAN_POINT('Ctrl Pts',(0.159106226437288,-1.,-1.98584238283279));
#22859=CARTESIAN_POINT('Ctrl Pts',(0.16062206078461,-1.,-1.97996195437557));
#22860=CARTESIAN_POINT('Ctrl Pts',(0.162079693556302,-1.,-1.97406280235204));
#22861=CARTESIAN_POINT('Ctrl Pts',(0.16347818545776,-1.,-1.96816512678));
#22862=CARTESIAN_POINT('Ctrl Pts',(0.1648165689203,-1.,-1.96229379940174));
#22863=CARTESIAN_POINT('Ctrl Pts',(0.166093592002833,-1.,-1.95646759718755));
#22864=CARTESIAN_POINT('Ctrl Pts',(0.167307501784469,-1.,-1.95069027794286));
#22865=CARTESIAN_POINT('Ctrl Pts',(0.168455741607516,-1.,-1.94493757756879));
#22866=CARTESIAN_POINT('Ctrl Pts',(0.169534904817425,-1.,-1.93915639211497));
#22867=CARTESIAN_POINT('Ctrl Pts',(0.170541253116136,-1.,-1.93329183155455));
#22868=CARTESIAN_POINT('Ctrl Pts',(0.17147119153296,-1.,-1.92731093582));
#22869=CARTESIAN_POINT('Ctrl Pts',(0.172321621259557,-1.,-1.92122334398034));
#22870=CARTESIAN_POINT('Ctrl Pts',(0.173090695383619,-1.,-1.91511429159681));
#22871=CARTESIAN_POINT('Ctrl Pts',(0.173776635257984,-1.,-1.90911693975475));
#22872=CARTESIAN_POINT('Ctrl Pts',(0.174375518661222,-1.,-1.90335253863003));
#22873=CARTESIAN_POINT('Ctrl Pts',(0.174879405091277,-1.,-1.89788101117148));
#22874=CARTESIAN_POINT('Ctrl Pts',(0.175274276190664,-1.,-1.89264630198279));
#22875=CARTESIAN_POINT('Ctrl Pts',(0.175538155840286,-1.,-1.88742606272818));
#22876=CARTESIAN_POINT('Ctrl Pts',(0.175644148889271,-1.,-1.88188663144846));
#22877=CARTESIAN_POINT('Ctrl Pts',(0.175563480746205,-1.,-1.87563767773249));
#22878=CARTESIAN_POINT('Ctrl Pts',(0.175268337590901,-1.,-1.86828349694972));
#22879=CARTESIAN_POINT('Ctrl Pts',(0.174735259276856,-1.,-1.85948367089838));
#22880=CARTESIAN_POINT('Ctrl Pts',(0.173946627589401,-1.,-1.84898113200543));
#22881=CARTESIAN_POINT('Ctrl Pts',(0.17288944289442,-1.,-1.83658380530747));
#22882=CARTESIAN_POINT('Ctrl Pts',(0.171554770207306,-1.,-1.82215766815414));
#22883=CARTESIAN_POINT('Ctrl Pts',(0.169936923908078,-1.,-1.80561530633924));
#22884=CARTESIAN_POINT('Ctrl Pts',(0.16803277280837,-1.,-1.78690649988931));
#22885=CARTESIAN_POINT('Ctrl Pts',(0.166279355148738,-1.,-1.77018771687692));
#22886=CARTESIAN_POINT('Ctrl Pts',(0.164834765708484,-1.,-1.75666056640041));
#22887=CARTESIAN_POINT('Ctrl Pts',(0.163814161002474,-1.,-1.74720349503904));
#22888=CARTESIAN_POINT('Ctrl Pts',(0.163289472382896,-1.,-1.74236521665491));
#22889=CARTESIAN_POINT('',(0.383122945602004,-1.,-1.7075470150345));
#22890=CARTESIAN_POINT('Origin',(0.,-1.,0.));
#22891=CARTESIAN_POINT('',(0.61342227326009,-1.,-2.11275013067528));
#22892=CARTESIAN_POINT('Ctrl Pts',(0.383122945602004,-1.,-1.7075470150345));
#22893=CARTESIAN_POINT('Ctrl Pts',(0.384119047314215,-1.,-1.71231062891398));
#22894=CARTESIAN_POINT('Ctrl Pts',(0.386070790323281,-1.,-1.72162022244582));
#22895=CARTESIAN_POINT('Ctrl Pts',(0.388877023502615,-1.,-1.73493170972829));
#22896=CARTESIAN_POINT('Ctrl Pts',(0.392375812285395,-1.,-1.75137405310193));
#22897=CARTESIAN_POINT('Ctrl Pts',(0.396346196110688,-1.,-1.76975560043442));
#22898=CARTESIAN_POINT('Ctrl Pts',(0.399919403774155,-1.,-1.78598826343754));
#22899=CARTESIAN_POINT('Ctrl Pts',(0.403107976163396,-1.,-1.80012077173238));
#22900=CARTESIAN_POINT('Ctrl Pts',(0.405933518407175,-1.,-1.81223801812013));
#22901=CARTESIAN_POINT('Ctrl Pts',(0.408428948106227,-1.,-1.82247022677562));
#22902=CARTESIAN_POINT('Ctrl Pts',(0.410641256301276,-1.,-1.83100408895047));
#22903=CARTESIAN_POINT('Ctrl Pts',(0.412633125322945,-1.,-1.8380895347617));
#22904=CARTESIAN_POINT('Ctrl Pts',(0.414487438255542,-1.,-1.84405757074218));
#22905=CARTESIAN_POINT('Ctrl Pts',(0.416300022039885,-1.,-1.84929312930314));
#22906=CARTESIAN_POINT('Ctrl Pts',(0.418164129144045,-1.,-1.8541763285645));
#22907=CARTESIAN_POINT('Ctrl Pts',(0.420157287975583,-1.,-1.8590328109667));
#22908=CARTESIAN_POINT('Ctrl Pts',(0.422327307417884,-1.,-1.86408083333863));
#22909=CARTESIAN_POINT('Ctrl Pts',(0.424678177290876,-1.,-1.8693780394412));
#22910=CARTESIAN_POINT('Ctrl Pts',(0.427183828518743,-1.,-1.87486989291334));
#22911=CARTESIAN_POINT('Ctrl Pts',(0.429803062482217,-1.,-1.88044229001779));
#22912=CARTESIAN_POINT('Ctrl Pts',(0.432493038548833,-1.,-1.88596913666828));
#22913=CARTESIAN_POINT('Ctrl Pts',(0.43522566096358,-1.,-1.89136993975585));
#22914=CARTESIAN_POINT('Ctrl Pts',(0.437995003948443,-1.,-1.89663648956549));
#22915=CARTESIAN_POINT('Ctrl Pts',(0.44080783370416,-1.,-1.90180124389137));
#22916=CARTESIAN_POINT('Ctrl Pts',(0.44367755684917,-1.,-1.90691756144906));
#22917=CARTESIAN_POINT('Ctrl Pts',(0.446617343485651,-1.,-1.91203699981095));
#22918=CARTESIAN_POINT('Ctrl Pts',(0.449632260106572,-1.,-1.91718342555717));
#22919=CARTESIAN_POINT('Ctrl Pts',(0.452719478359356,-1.,-1.9223538064847));
#22920=CARTESIAN_POINT('Ctrl Pts',(0.455872005174335,-1.,-1.92753067150461));
#22921=CARTESIAN_POINT('Ctrl Pts',(0.459081234547931,-1.,-1.93269066517936));
#22922=CARTESIAN_POINT('Ctrl Pts',(0.462340031009087,-1.,-1.93781486640834));
#22923=CARTESIAN_POINT('Ctrl Pts',(0.465645462026064,-1.,-1.94289794196205));
#22924=CARTESIAN_POINT('Ctrl Pts',(0.468997482913158,-1.,-1.94794381136524));
#22925=CARTESIAN_POINT('Ctrl Pts',(0.472397672264079,-1.,-1.95296148278136));
#22926=CARTESIAN_POINT('Ctrl Pts',(0.475848034683171,-1.,-1.95796111148175));
#22927=CARTESIAN_POINT('Ctrl Pts',(0.479349583074846,-1.,-1.96294933055938));
#22928=CARTESIAN_POINT('Ctrl Pts',(0.482901662120686,-1.,-1.96792703422358));
#22929=CARTESIAN_POINT('Ctrl Pts',(0.486502692907661,-1.,-1.97289186263272));
#22930=CARTESIAN_POINT('Ctrl Pts',(0.490150627860955,-1.,-1.97783973019229));
#22931=CARTESIAN_POINT('Ctrl Pts',(0.493843476541492,-1.,-1.9827665876182));
#22932=CARTESIAN_POINT('Ctrl Pts',(0.497579909545564,-1.,-1.98767044752929));
#22933=CARTESIAN_POINT('Ctrl Pts',(0.501359287727129,-1.,-1.9925514912615));
#22934=CARTESIAN_POINT('Ctrl Pts',(0.505181361323011,-1.,-1.99741107463567));
#22935=CARTESIAN_POINT('Ctrl Pts',(0.509046069886152,-1.,-2.00225107134733));
#22936=CARTESIAN_POINT('Ctrl Pts',(0.512953306961813,-1.,-2.00707309946955));
#22937=CARTESIAN_POINT('Ctrl Pts',(0.516902681728733,-1.,-2.01187773939257));
#22938=CARTESIAN_POINT('Ctrl Pts',(0.520893590399428,-1.,-2.01666477917306));
#22939=CARTESIAN_POINT('Ctrl Pts',(0.524925318333518,-1.,-2.02143356304712));
#22940=CARTESIAN_POINT('Ctrl Pts',(0.52899712724191,-1.,-2.02618329083289));
#22941=CARTESIAN_POINT('Ctrl Pts',(0.533108355132905,-1.,-2.03091336214401));
#22942=CARTESIAN_POINT('Ctrl Pts',(0.537258489833134,-1.,-2.03562362953993));
#22943=CARTESIAN_POINT('Ctrl Pts',(0.54144712061552,-1.,-2.0403142269048));
#22944=CARTESIAN_POINT('Ctrl Pts',(0.545673903817348,-1.,-2.0449854471456));
#22945=CARTESIAN_POINT('Ctrl Pts',(0.549938525150342,-1.,-2.04963761077974));
#22946=CARTESIAN_POINT('Ctrl Pts',(0.554240657464109,-1.,-2.05427091604482));
#22947=CARTESIAN_POINT('Ctrl Pts',(0.558579940185467,-1.,-2.05888537756571));
#22948=CARTESIAN_POINT('Ctrl Pts',(0.562955993082574,-1.,-2.06348090160697));
#22949=CARTESIAN_POINT('Ctrl Pts',(0.567368421181229,-1.,-2.06805732997383));
#22950=CARTESIAN_POINT('Ctrl Pts',(0.571816823242411,-1.,-2.07261449292758));
#22951=CARTESIAN_POINT('Ctrl Pts',(0.576300797416274,-1.,-2.07715226767361));
#22952=CARTESIAN_POINT('Ctrl Pts',(0.580819952107256,-1.,-2.08167059018138));
#22953=CARTESIAN_POINT('Ctrl Pts',(0.585373918990895,-1.,-2.086169437277));
#22954=CARTESIAN_POINT('Ctrl Pts',(0.589962365403189,-1.,-2.09064881812053));
#22955=CARTESIAN_POINT('Ctrl Pts',(0.594585006052823,-1.,-2.09510876220501));
#22956=CARTESIAN_POINT('Ctrl Pts',(0.599241616422144,-1.,-2.09954930865331));
#22957=CARTESIAN_POINT('Ctrl Pts',(0.603932030738212,-1.,-2.10397049887709));
#22958=CARTESIAN_POINT('Ctrl Pts',(0.607711315456826,-1.,-2.10749199615859));
#22959=CARTESIAN_POINT('Ctrl Pts',(0.610560911691113,-1.,-2.11012443807661));
#22960=CARTESIAN_POINT('Ctrl Pts',(0.61246736556225,-1.,-2.11187554260142));
#22961=CARTESIAN_POINT('Ctrl Pts',(0.61342227326009,-1.,-2.11275013067528));
#22962=CARTESIAN_POINT('',(0.745574324794401,-1.,-2.0698113262342));
#22963=CARTESIAN_POINT('',(0.61342227326009,-1.,-2.11275013067528));
#22964=CARTESIAN_POINT('',(0.693717979106306,-1.,-1.60662857109684));
#22965=CARTESIAN_POINT('Ctrl Pts',(0.745574324794401,-1.,-2.0698113262342));
#22966=CARTESIAN_POINT('Ctrl Pts',(0.74583279137781,-1.,-2.06854248895575));
#22967=CARTESIAN_POINT('Ctrl Pts',(0.746345871542695,-1.,-2.06600523016401));
#22968=CARTESIAN_POINT('Ctrl Pts',(0.747103932785504,-1.,-2.06220058927162));
#22969=CARTESIAN_POINT('Ctrl Pts',(0.748091554181101,-1.,-2.05713023030263));
#22970=CARTESIAN_POINT('Ctrl Pts',(0.749287468663053,-1.,-2.05079645591606));
#22971=CARTESIAN_POINT('Ctrl Pts',(0.750444657874758,-1.,-2.04446689147754));
#22972=CARTESIAN_POINT('Ctrl Pts',(0.751562963361383,-1.,-2.03814160092173));
#22973=CARTESIAN_POINT('Ctrl Pts',(0.752642180488104,-1.,-2.03182068456467));
#22974=CARTESIAN_POINT('Ctrl Pts',(0.753682061113765,-1.,-2.02550428623587));
#22975=CARTESIAN_POINT('Ctrl Pts',(0.75468233072352,-1.,-2.01919259406003));
#22976=CARTESIAN_POINT('Ctrl Pts',(0.7556427049581,-1.,-2.01288584328149));
#22977=CARTESIAN_POINT('Ctrl Pts',(0.756562904646496,-1.,-2.00658431587682));
#22978=CARTESIAN_POINT('Ctrl Pts',(0.757442676862341,-1.,-2.00028834739072));
#22979=CARTESIAN_POINT('Ctrl Pts',(0.758281796766377,-1.,-1.9939983109871));
#22980=CARTESIAN_POINT('Ctrl Pts',(0.759080037802242,-1.,-1.98771456680806));
#22981=CARTESIAN_POINT('Ctrl Pts',(0.759837147452135,-1.,-1.98143741418156));
#22982=CARTESIAN_POINT('Ctrl Pts',(0.760552825409855,-1.,-1.97516705321521));
#22983=CARTESIAN_POINT('Ctrl Pts',(0.761226690483986,-1.,-1.96890351582545));
#22984=CARTESIAN_POINT('Ctrl Pts',(0.761858300014575,-1.,-1.96264672744229));
#22985=CARTESIAN_POINT('Ctrl Pts',(0.762447203806263,-1.,-1.95639665309893));
#22986=CARTESIAN_POINT('Ctrl Pts',(0.762992990878774,-1.,-1.95015342590025));
#22987=CARTESIAN_POINT('Ctrl Pts',(0.76349533353858,-1.,-1.94391746617626));
#22988=CARTESIAN_POINT('Ctrl Pts',(0.763954049121393,-1.,-1.93768964875867));
#22989=CARTESIAN_POINT('Ctrl Pts',(0.764369010673889,-1.,-1.93147105496367));
#22990=CARTESIAN_POINT('Ctrl Pts',(0.764740025488189,-1.,-1.92526263537041));
#22991=CARTESIAN_POINT('Ctrl Pts',(0.765066729667095,-1.,-1.91906491634197));
#22992=CARTESIAN_POINT('Ctrl Pts',(0.765348465884739,-1.,-1.91287765805174));
#22993=CARTESIAN_POINT('Ctrl Pts',(0.765584196937936,-1.,-1.90669961402362));
#22994=CARTESIAN_POINT('Ctrl Pts',(0.765772772593395,-1.,-1.90052930393599));
#22995=CARTESIAN_POINT('Ctrl Pts',(0.765913193856979,-1.,-1.89436577771389));
#22996=CARTESIAN_POINT('Ctrl Pts',(0.76600483706209,-1.,-1.88820926433409));
#22997=CARTESIAN_POINT('Ctrl Pts',(0.766047794851868,-1.,-1.88206215302561));
#22998=CARTESIAN_POINT('Ctrl Pts',(0.766042837036759,-1.,-1.87592888967886));
#22999=CARTESIAN_POINT('Ctrl Pts',(0.765990708546111,-1.,-1.86981398314345));
#23000=CARTESIAN_POINT('Ctrl Pts',(0.765891519092557,-1.,-1.86372027063315));
#23001=CARTESIAN_POINT('Ctrl Pts',(0.765744212909305,-1.,-1.85764741390391));
#23002=CARTESIAN_POINT('Ctrl Pts',(0.765545710619023,-1.,-1.85158945130054));
#23003=CARTESIAN_POINT('Ctrl Pts',(0.765291664861971,-1.,-1.84553698875911));
#23004=CARTESIAN_POINT('Ctrl Pts',(0.764978057881687,-1.,-1.83948181064823));
#23005=CARTESIAN_POINT('Ctrl Pts',(0.764602549687845,-1.,-1.8334207722714));
#23006=CARTESIAN_POINT('Ctrl Pts',(0.764165902606055,-1.,-1.8273599120008));
#23007=CARTESIAN_POINT('Ctrl Pts',(0.763673465462854,-1.,-1.82131873145297));
#23008=CARTESIAN_POINT('Ctrl Pts',(0.763132003836783,-1.,-1.81532118405566));
#23009=CARTESIAN_POINT('Ctrl Pts',(0.762546129464036,-1.,-1.80938551463989));
#23010=CARTESIAN_POINT('Ctrl Pts',(0.761915336443515,-1.,-1.80351583877334));
#23011=CARTESIAN_POINT('Ctrl Pts',(0.761229695230359,-1.,-1.79768986997735));
#23012=CARTESIAN_POINT('Ctrl Pts',(0.760469555880425,-1.,-1.79185815610802));
#23013=CARTESIAN_POINT('Ctrl Pts',(0.759614401109868,-1.,-1.78596964884527));
#23014=CARTESIAN_POINT('Ctrl Pts',(0.75865062667738,-1.,-1.77999411220912));
#23015=CARTESIAN_POINT('Ctrl Pts',(0.757578264077238,-1.,-1.77394167108342));
#23016=CARTESIAN_POINT('Ctrl Pts',(0.756421896028403,-1.,-1.76789396003141));
#23017=CARTESIAN_POINT('Ctrl Pts',(0.755220979975262,-1.,-1.7619781724032));
#23018=CARTESIAN_POINT('Ctrl Pts',(0.75400925402848,-1.,-1.75631083600175));
#23019=CARTESIAN_POINT('Ctrl Pts',(0.752797683531377,-1.,-1.75095139468809));
#23020=CARTESIAN_POINT('Ctrl Pts',(0.751555614163629,-1.,-1.74585086852298));
#23021=CARTESIAN_POINT('Ctrl Pts',(0.75019343597954,-1.,-1.74080458266705));
#23022=CARTESIAN_POINT('Ctrl Pts',(0.748582462954854,-1.,-1.73550351679848));
#23023=CARTESIAN_POINT('Ctrl Pts',(0.746574710096436,-1.,-1.72958533647399));
#23024=CARTESIAN_POINT('Ctrl Pts',(0.744021445433764,-1.,-1.7226822991693));
#23025=CARTESIAN_POINT('Ctrl Pts',(0.740795162032087,-1.,-1.71447789751927));
#23026=CARTESIAN_POINT('Ctrl Pts',(0.736799665724771,-1.,-1.70473309006121));
#23027=CARTESIAN_POINT('Ctrl Pts',(0.731963238697195,-1.,-1.69326921975743));
#23028=CARTESIAN_POINT('Ctrl Pts',(0.726235967997433,-1.,-1.67996158455503));
#23029=CARTESIAN_POINT('Ctrl Pts',(0.719585433804282,-1.,-1.6647288055568));
#23030=CARTESIAN_POINT('Ctrl Pts',(0.711993139355394,-1.,-1.64752408832016));
#23031=CARTESIAN_POINT('Ctrl Pts',(0.705159151988319,-1.,-1.63216541664676));
#23032=CARTESIAN_POINT('Ctrl Pts',(0.699605146405088,-1.,-1.61974673472612));
#23033=CARTESIAN_POINT('Ctrl Pts',(0.695712097881194,-1.,-1.61106790958151));
#23034=CARTESIAN_POINT('Ctrl Pts',(0.693717979106306,-1.,-1.60662857109684));
#23035=CARTESIAN_POINT('',(0.892032620296855,-1.,-1.5055822144029));
#23036=CARTESIAN_POINT('Origin',(0.,-1.,0.));
#23037=CARTESIAN_POINT('',(1.23627494547115,-1.,-1.81978687191668));
#23038=CARTESIAN_POINT('Ctrl Pts',(0.892032620296855,-1.,-1.5055822144029));
#23039=CARTESIAN_POINT('Ctrl Pts',(0.894452006964543,-1.,-1.50980486806688));
#23040=CARTESIAN_POINT('Ctrl Pts',(0.89918504748351,-1.,-1.51805569590094));
#23041=CARTESIAN_POINT('Ctrl Pts',(0.905967409625651,-1.,-1.52984849887993));
#23042=CARTESIAN_POINT('Ctrl Pts',(0.914375919026456,-1.,-1.54440491149498));
#23043=CARTESIAN_POINT('Ctrl Pts',(0.923832188944341,-1.,-1.56065988578893));
#23044=CARTESIAN_POINT('Ctrl Pts',(0.932246680108685,-1.,-1.57499388382243));
#23045=CARTESIAN_POINT('Ctrl Pts',(0.939646377893399,-1.,-1.58744937487176));
#23046=CARTESIAN_POINT('Ctrl Pts',(0.946078063315257,-1.,-1.59810042043673));
#23047=CARTESIAN_POINT('Ctrl Pts',(0.951613284356035,-1.,-1.60706069896936));
#23048=CARTESIAN_POINT('Ctrl Pts',(0.95635442292067,-1.,-1.61449324337085));
#23049=CARTESIAN_POINT('Ctrl Pts',(0.960438326101728,-1.,-1.62061638140221));
#23050=CARTESIAN_POINT('Ctrl Pts',(0.964046107040535,-1.,-1.62571930670187));
#23051=CARTESIAN_POINT('Ctrl Pts',(0.967387853230345,-1.,-1.63013849959462));
#23052=CARTESIAN_POINT('Ctrl Pts',(0.970669715997509,-1.,-1.63420665729798));
#23053=CARTESIAN_POINT('Ctrl Pts',(0.974066058287418,-1.,-1.63820952658144));
#23054=CARTESIAN_POINT('Ctrl Pts',(0.977689794119416,-1.,-1.64233990826687));
#23055=CARTESIAN_POINT('Ctrl Pts',(0.981562530939489,-1.,-1.64665139190656));
#23056=CARTESIAN_POINT('Ctrl Pts',(0.98564262292082,-1.,-1.65110016612638));
#23057=CARTESIAN_POINT('Ctrl Pts',(0.989855627854164,-1.,-1.65559044289699));
#23058=CARTESIAN_POINT('Ctrl Pts',(0.994121836661305,-1.,-1.66001553809947));
#23059=CARTESIAN_POINT('Ctrl Pts',(0.998389654952757,-1.,-1.66430758030376));
#23060=CARTESIAN_POINT('Ctrl Pts',(1.00265091003727,-1.,-1.66846059277303));
#23061=CARTESIAN_POINT('Ctrl Pts',(1.00692206696414,-1.,-1.67250335383293));
#23062=CARTESIAN_POINT('Ctrl Pts',(1.01123236493511,-1.,-1.67648246776464));
#23063=CARTESIAN_POINT('Ctrl Pts',(1.01561026162773,-1.,-1.68044289894798));
#23064=CARTESIAN_POINT('Ctrl Pts',(1.02006795074201,-1.,-1.68440578021706));
#23065=CARTESIAN_POINT('Ctrl Pts',(1.02460180535255,-1.,-1.68836910178447));
#23066=CARTESIAN_POINT('Ctrl Pts',(1.02919977579147,-1.,-1.69231840863458));
#23067=CARTESIAN_POINT('Ctrl Pts',(1.03384646003588,-1.,-1.69623414782771));
#23068=CARTESIAN_POINT('Ctrl Pts',(1.03852922490789,-1.,-1.70010052930962));
#23069=CARTESIAN_POINT('Ctrl Pts',(1.04324363334554,-1.,-1.70391338707982));
#23070=CARTESIAN_POINT('Ctrl Pts',(1.04799085404995,-1.,-1.70767646263649));
#23071=CARTESIAN_POINT('Ctrl Pts',(1.05277517202855,-1.,-1.71139783543989));
#23072=CARTESIAN_POINT('Ctrl Pts',(1.05760163192479,-1.,-1.7150865442702));
#23073=CARTESIAN_POINT('Ctrl Pts',(1.06247324680647,-1.,-1.71874858456904));
#23074=CARTESIAN_POINT('Ctrl Pts',(1.06738966975462,-1.,-1.72238500928453));
#23075=CARTESIAN_POINT('Ctrl Pts',(1.07234866990252,-1.,-1.72599406198488));
#23076=CARTESIAN_POINT('Ctrl Pts',(1.0773470373727,-1.,-1.72957248977424));
#23077=CARTESIAN_POINT('Ctrl Pts',(1.08238162784749,-1.,-1.73311705663407));
#23078=CARTESIAN_POINT('Ctrl Pts',(1.08745056285427,-1.,-1.73662628326091));
#23079=CARTESIAN_POINT('Ctrl Pts',(1.09255329056493,-1.,-1.74010053962247));
#23080=CARTESIAN_POINT('Ctrl Pts',(1.09768999241225,-1.,-1.74354119236208));
#23081=CARTESIAN_POINT('Ctrl Pts',(1.10286118991143,-1.,-1.74695004214923));
#23082=CARTESIAN_POINT('Ctrl Pts',(1.10806728183007,-1.,-1.7503286607592));
#23083=CARTESIAN_POINT('Ctrl Pts',(1.11330807582551,-1.,-1.7536777209463));
#23084=CARTESIAN_POINT('Ctrl Pts',(1.11858293216763,-1.,-1.75699720772105));
#23085=CARTESIAN_POINT('Ctrl Pts',(1.12389096855086,-1.,-1.76028671825096));
#23086=CARTESIAN_POINT('Ctrl Pts',(1.12923123555075,-1.,-1.7635457196617));
#23087=CARTESIAN_POINT('Ctrl Pts',(1.1346029180462,-1.,-1.76677384551862));
#23088=CARTESIAN_POINT('Ctrl Pts',(1.14000548336975,-1.,-1.76997111386769));
#23089=CARTESIAN_POINT('Ctrl Pts',(1.1454385822692,-1.,-1.77313777896194));
#23090=CARTESIAN_POINT('Ctrl Pts',(1.15090197841514,-1.,-1.7762742255701));
#23091=CARTESIAN_POINT('Ctrl Pts',(1.15639547194698,-1.,-1.77938085564275));
#23092=CARTESIAN_POINT('Ctrl Pts',(1.16191881298499,-1.,-1.78245795881009));
#23093=CARTESIAN_POINT('Ctrl Pts',(1.16747166312303,-1.,-1.78550566040443));
#23094=CARTESIAN_POINT('Ctrl Pts',(1.17305363177328,-1.,-1.78852398877617));
#23095=CARTESIAN_POINT('Ctrl Pts',(1.17866429440809,-1.,-1.79151291552689));
#23096=CARTESIAN_POINT('Ctrl Pts',(1.18430321697432,-1.,-1.79447240321515));
#23097=CARTESIAN_POINT('Ctrl Pts',(1.18996997934445,-1.,-1.79740245923478));
#23098=CARTESIAN_POINT('Ctrl Pts',(1.19566418930242,-1.,-1.80030314369879));
#23099=CARTESIAN_POINT('Ctrl Pts',(1.20138548938974,-1.,-1.80317454838603));
#23100=CARTESIAN_POINT('Ctrl Pts',(1.20713356605475,-1.,-1.80601678480707));
#23101=CARTESIAN_POINT('Ctrl Pts',(1.21290815708314,-1.,-1.80882996917129));
#23102=CARTESIAN_POINT('Ctrl Pts',(1.21870906103557,-1.,-1.81161420806656));
#23103=CARTESIAN_POINT('Ctrl Pts',(1.2245361330495,-1.,-1.81436959210434));
#23104=CARTESIAN_POINT('Ctrl Pts',(1.2292186489137,-1.,-1.8165508718364));
#23105=CARTESIAN_POINT('Ctrl Pts',(1.2327422452705,-1.,-1.81817389921279));
#23106=CARTESIAN_POINT('Ctrl Pts',(1.23509651170476,-1.,-1.81925017193666));
#23107=CARTESIAN_POINT('Ctrl Pts',(1.23627494547115,-1.,-1.81978687191668));
#23108=CARTESIAN_POINT('',(1.34869019493419,-1.,-1.73811241238545));
#23109=CARTESIAN_POINT('',(1.23627494547115,-1.,-1.81978687191668));
#23110=CARTESIAN_POINT('',(1.15624053661742,-1.,-1.31362392696032));
#23111=CARTESIAN_POINT('Ctrl Pts',(1.34869019493419,-1.,-1.73811241238545));
#23112=CARTESIAN_POINT('Ctrl Pts',(1.34854391898045,-1.,-1.73682580585691));
#23113=CARTESIAN_POINT('Ctrl Pts',(1.34824783112887,-1.,-1.73425417885907));
#23114=CARTESIAN_POINT('Ctrl Pts',(1.34779309152035,-1.,-1.7304014965394));
#23115=CARTESIAN_POINT('Ctrl Pts',(1.34716554819527,-1.,-1.72527410680674));
#23116=CARTESIAN_POINT('Ctrl Pts',(1.34634568653227,-1.,-1.7188807715049));
#23117=CARTESIAN_POINT('Ctrl Pts',(1.34549029589416,-1.,-1.71250340686822));
#23118=CARTESIAN_POINT('Ctrl Pts',(1.34459924533831,-1.,-1.70614212266738));
#23119=CARTESIAN_POINT('Ctrl Pts',(1.34367237124483,-1.,-1.69979707754427));
#23120=CARTESIAN_POINT('Ctrl Pts',(1.34270948206319,-1.,-1.6934684849687));
#23121=CARTESIAN_POINT('Ctrl Pts',(1.341710374848,-1.,-1.68715660868764));
#23122=CARTESIAN_POINT('Ctrl Pts',(1.34067485185203,-1.,-1.68086176030362));
#23123=CARTESIAN_POINT('Ctrl Pts',(1.3396027347034,-1.,-1.67458429426086));
#23124=CARTESIAN_POINT('Ctrl Pts',(1.33849388654388,-1.,-1.66832460783989));
#23125=CARTESIAN_POINT('Ctrl Pts',(1.33734820885262,-1.,-1.66208312541983));
#23126=CARTESIAN_POINT('Ctrl Pts',(1.33616559745172,-1.,-1.65586025952593));
#23127=CARTESIAN_POINT('Ctrl Pts',(1.33494590467993,-1.,-1.6496563728683));
#23128=CARTESIAN_POINT('Ctrl Pts',(1.33368890676572,-1.,-1.6434717485603));
#23129=CARTESIAN_POINT('Ctrl Pts',(1.33239425103724,-1.,-1.63730653475089));
#23130=CARTESIAN_POINT('Ctrl Pts',(1.33106149345645,-1.,-1.63116079730923));
#23131=CARTESIAN_POINT('Ctrl Pts',(1.3296901950568,-1.,-1.62503464209797));
#23132=CARTESIAN_POINT('Ctrl Pts',(1.32828000610449,-1.,-1.61892832270724));
#23133=CARTESIAN_POINT('Ctrl Pts',(1.32683074483356,-1.,-1.6128423401575));
#23134=CARTESIAN_POINT('Ctrl Pts',(1.32534250785782,-1.,-1.60677758290954));
#23135=CARTESIAN_POINT('Ctrl Pts',(1.32381550858256,-1.,-1.60073511858687));
#23136=CARTESIAN_POINT('Ctrl Pts',(1.32224985747682,-1.,-1.59471591079403));
#23137=CARTESIAN_POINT('Ctrl Pts',(1.32064537110892,-1.,-1.58872057258245));
#23138=CARTESIAN_POINT('Ctrl Pts',(1.31900135021432,-1.,-1.58274907898834));
#23139=CARTESIAN_POINT('Ctrl Pts',(1.31731642317187,-1.,-1.5768005650559));
#23140=CARTESIAN_POINT('Ctrl Pts',(1.31558903860016,-1.,-1.57087397835723));
#23141=CARTESIAN_POINT('Ctrl Pts',(1.31381795281002,-1.,-1.56496872402353));
#23142=CARTESIAN_POINT('Ctrl Pts',(1.31200264341696,-1.,-1.55908521254821));
#23143=CARTESIAN_POINT('Ctrl Pts',(1.31014393684222,-1.,-1.55322568759481));
#23144=CARTESIAN_POINT('Ctrl Pts',(1.30824393907473,-1.,-1.54739413957185));
#23145=CARTESIAN_POINT('Ctrl Pts',(1.30630475189556,-1.,-1.54159462645432));
#23146=CARTESIAN_POINT('Ctrl Pts',(1.30432735639489,-1.,-1.53582981268977));
#23147=CARTESIAN_POINT('Ctrl Pts',(1.30231064395568,-1.,-1.53009970283891));
#23148=CARTESIAN_POINT('Ctrl Pts',(1.30024984366328,-1.,-1.52439957861062));
#23149=CARTESIAN_POINT('Ctrl Pts',(1.29813791800747,-1.,-1.51872184912724));
#23150=CARTESIAN_POINT('Ctrl Pts',(1.29596850710509,-1.,-1.51305994241402));
#23151=CARTESIAN_POINT('Ctrl Pts',(1.29373841372842,-1.,-1.50741159078365));
#23152=CARTESIAN_POINT('Ctrl Pts',(1.29145022885181,-1.,-1.50178230149776));
#23153=CARTESIAN_POINT('Ctrl Pts',(1.28911506584254,-1.,-1.49618896881754));
#23154=CARTESIAN_POINT('Ctrl Pts',(1.2867467611644,-1.,-1.4906522831278));
#23155=CARTESIAN_POINT('Ctrl Pts',(1.28435533880201,-1.,-1.4851881711891));
#23156=CARTESIAN_POINT('Ctrl Pts',(1.28194158939517,-1.,-1.47980070347096));
#23157=CARTESIAN_POINT('Ctrl Pts',(1.2794891824849,-1.,-1.4744717526707));
#23158=CARTESIAN_POINT('Ctrl Pts',(1.27696414831089,-1.,-1.46916035917133));
#23159=CARTESIAN_POINT('Ctrl Pts',(1.27433119897822,-1.,-1.46382431332476));
#23160=CARTESIAN_POINT('Ctrl Pts',(1.27156805265289,-1.,-1.45843906294697));
#23161=CARTESIAN_POINT('Ctrl Pts',(1.2686778680489,-1.,-1.45301422764247));
#23162=CARTESIAN_POINT('Ctrl Pts',(1.26570925118868,-1.,-1.44761985001662));
#23163=CARTESIAN_POINT('Ctrl Pts',(1.26273903323858,-1.,-1.44236470511303));
#23164=CARTESIAN_POINT('Ctrl Pts',(1.25983531012005,-1.,-1.43734919180848));
#23165=CARTESIAN_POINT('Ctrl Pts',(1.25702687965755,-1.,-1.43262645609691));
#23166=CARTESIAN_POINT('Ctrl Pts',(1.25426945222639,-1.,-1.42815938799387));
#23167=CARTESIAN_POINT('Ctrl Pts',(1.2514145557001,-1.,-1.42378102115575));
#23168=CARTESIAN_POINT('Ctrl Pts',(1.24824430986571,-1.,-1.41923722596025));
#23169=CARTESIAN_POINT('Ctrl Pts',(1.24450600513056,-1.,-1.41422913175179));
#23170=CARTESIAN_POINT('Ctrl Pts',(1.23994455029534,-1.,-1.40845295531283));
#23171=CARTESIAN_POINT('Ctrl Pts',(1.23434087290423,-1.,-1.40164708206106));
#23172=CARTESIAN_POINT('Ctrl Pts',(1.22752961899387,-1.,-1.39361389568796));
#23173=CARTESIAN_POINT('Ctrl Pts',(1.21938737280852,-1.,-1.38420564527715));
#23174=CARTESIAN_POINT('Ctrl Pts',(1.20982812925645,-1.,-1.37331915607905));
#23175=CARTESIAN_POINT('Ctrl Pts',(1.1987959077932,-1.,-1.36088705043885));
#23176=CARTESIAN_POINT('Ctrl Pts',(1.18625865667441,-1.,-1.34687054001093));
#23177=CARTESIAN_POINT('Ctrl Pts',(1.17501305789857,-1.,-1.33437539347008));
#23178=CARTESIAN_POINT('Ctrl Pts',(1.16589330093588,-1.,-1.32428080721772));
#23179=CARTESIAN_POINT('Ctrl Pts',(1.15950888730809,-1.,-1.31722977216397));
#23180=CARTESIAN_POINT('Ctrl Pts',(1.15624053661742,-1.,-1.31362392696032));
#23181=CARTESIAN_POINT('',(1.31362392696032,-1.,-1.15624053661742));
#23182=CARTESIAN_POINT('Origin',(0.,-1.,0.));
#23183=CARTESIAN_POINT('',(1.73811241238545,-1.,-1.34869019493419));
#23184=CARTESIAN_POINT('Ctrl Pts',(1.31362392696032,-1.,-1.15624053661742));
#23185=CARTESIAN_POINT('Ctrl Pts',(1.3172297721596,-1.,-1.15950888730433));
#23186=CARTESIAN_POINT('Ctrl Pts',(1.32428080720544,-1.,-1.16589330092532));
#23187=CARTESIAN_POINT('Ctrl Pts',(1.33437539344842,-1.,-1.17501305787994));
#23188=CARTESIAN_POINT('Ctrl Pts',(1.34687053998157,-1.,-1.18625865664915));
#23189=CARTESIAN_POINT('Ctrl Pts',(1.36088705040677,-1.,-1.1987959077656));
#23190=CARTESIAN_POINT('Ctrl Pts',(1.37331915604962,-1.,-1.20982812923113));
#23191=CARTESIAN_POINT('Ctrl Pts',(1.38420564525391,-1.,-1.21938737278853));
#23192=CARTESIAN_POINT('Ctrl Pts',(1.39361389567257,-1.,-1.22752961898063));
#23193=CARTESIAN_POINT('Ctrl Pts',(1.40164708205345,-1.,-1.23434087289768));
#23194=CARTESIAN_POINT('Ctrl Pts',(1.40845295531151,-1.,-1.23994455029421));
#23195=CARTESIAN_POINT('Ctrl Pts',(1.41422913175437,-1.,-1.24450600513278));
#23196=CARTESIAN_POINT('Ctrl Pts',(1.41923722596421,-1.,-1.24824430986911));
#23197=CARTESIAN_POINT('Ctrl Pts',(1.42378102115911,-1.,-1.25141455570299));
#23198=CARTESIAN_POINT('Ctrl Pts',(1.42815938799555,-1.,-1.25426945222783));
#23199=CARTESIAN_POINT('Ctrl Pts',(1.43262645609679,-1.,-1.25702687965744));
#23200=CARTESIAN_POINT('Ctrl Pts',(1.43734919180719,-1.,-1.25983531011894));
#23201=CARTESIAN_POINT('Ctrl Pts',(1.44236470511145,-1.,-1.26273903323723));
#23202=CARTESIAN_POINT('Ctrl Pts',(1.44761985001544,-1.,-1.26570925118767));
#23203=CARTESIAN_POINT('Ctrl Pts',(1.45301422764205,-1.,-1.26867786804854));
#23204=CARTESIAN_POINT('Ctrl Pts',(1.45843906294725,-1.,-1.27156805265312));
#23205=CARTESIAN_POINT('Ctrl Pts',(1.4638243133254,-1.,-1.27433119897877));
#23206=CARTESIAN_POINT('Ctrl Pts',(1.46916035917197,-1.,-1.27696414831144));
#23207=CARTESIAN_POINT('Ctrl Pts',(1.4744717526711,-1.,-1.27948918248524));
#23208=CARTESIAN_POINT('Ctrl Pts',(1.47980070347102,-1.,-1.28194158939522));
#23209=CARTESIAN_POINT('Ctrl Pts',(1.48518817118891,-1.,-1.28435533880184));
#23210=CARTESIAN_POINT('Ctrl Pts',(1.4906522831275,-1.,-1.28674676116415));
#23211=CARTESIAN_POINT('Ctrl Pts',(1.49618896881729,-1.,-1.28911506584232));
#23212=CARTESIAN_POINT('Ctrl Pts',(1.50178230149764,-1.,-1.29145022885171));
#23213=CARTESIAN_POINT('Ctrl Pts',(1.50741159078367,-1.,-1.29373841372843));
#23214=CARTESIAN_POINT('Ctrl Pts',(1.51305994241412,-1.,-1.29596850710518));
#23215=CARTESIAN_POINT('Ctrl Pts',(1.51872184912735,-1.,-1.29813791800757));
#23216=CARTESIAN_POINT('Ctrl Pts',(1.5243995786107,-1.,-1.30024984366334));
#23217=CARTESIAN_POINT('Ctrl Pts',(1.53009970283893,-1.,-1.3023106439557));
#23218=CARTESIAN_POINT('Ctrl Pts',(1.53582981268976,-1.,-1.30432735639487));
#23219=CARTESIAN_POINT('Ctrl Pts',(1.54159462645428,-1.,-1.30630475189553));
#23220=CARTESIAN_POINT('Ctrl Pts',(1.54739413957183,-1.,-1.30824393907471));
#23221=CARTESIAN_POINT('Ctrl Pts',(1.55322568759481,-1.,-1.31014393684221));
#23222=CARTESIAN_POINT('Ctrl Pts',(1.55908521254822,-1.,-1.31200264341696));
#23223=CARTESIAN_POINT('Ctrl Pts',(1.56496872402352,-1.,-1.31381795281002));
#23224=CARTESIAN_POINT('Ctrl Pts',(1.57087397835721,-1.,-1.31558903860015));
#23225=CARTESIAN_POINT('Ctrl Pts',(1.57680056505585,-1.,-1.31731642317183));
#23226=CARTESIAN_POINT('Ctrl Pts',(1.58274907898829,-1.,-1.31900135021428));
#23227=CARTESIAN_POINT('Ctrl Pts',(1.58872057258244,-1.,-1.32064537110891));
#23228=CARTESIAN_POINT('Ctrl Pts',(1.59471591079408,-1.,-1.32224985747686));
#23229=CARTESIAN_POINT('Ctrl Pts',(1.600735118587,-1.,-1.32381550858266));
#23230=CARTESIAN_POINT('Ctrl Pts',(1.6067775829097,-1.,-1.32534250785794));
#23231=CARTESIAN_POINT('Ctrl Pts',(1.61284234015762,-1.,-1.32683074483365));
#23232=CARTESIAN_POINT('Ctrl Pts',(1.61892832270723,-1.,-1.32828000610448));
#23233=CARTESIAN_POINT('Ctrl Pts',(1.62503464209777,-1.,-1.32969019505665));
#23234=CARTESIAN_POINT('Ctrl Pts',(1.63116079730887,-1.,-1.33106149345618));
#23235=CARTESIAN_POINT('Ctrl Pts',(1.63730653475049,-1.,-1.33239425103694));
#23236=CARTESIAN_POINT('Ctrl Pts',(1.64347174856007,-1.,-1.33368890676554));
#23237=CARTESIAN_POINT('Ctrl Pts',(1.64965637286843,-1.,-1.33494590468003));
#23238=CARTESIAN_POINT('Ctrl Pts',(1.65586025952651,-1.,-1.33616559745217));
#23239=CARTESIAN_POINT('Ctrl Pts',(1.66208312542073,-1.,-1.33734820885331));
#23240=CARTESIAN_POINT('Ctrl Pts',(1.66832460784078,-1.,-1.33849388654458));
#23241=CARTESIAN_POINT('Ctrl Pts',(1.67458429426126,-1.,-1.33960273470372));
#23242=CARTESIAN_POINT('Ctrl Pts',(1.68086176030308,-1.,-1.3406748518516));
#23243=CARTESIAN_POINT('Ctrl Pts',(1.68715660868602,-1.,-1.34171037484673));
#23244=CARTESIAN_POINT('Ctrl Pts',(1.6934684849664,-1.,-1.34270948206139));
#23245=CARTESIAN_POINT('Ctrl Pts',(1.69979707754221,-1.,-1.34367237124322));
#23246=CARTESIAN_POINT('Ctrl Pts',(1.70614212266676,-1.,-1.34459924533783));
#23247=CARTESIAN_POINT('Ctrl Pts',(1.71250340687011,-1.,-1.34549029589563));
#23248=CARTESIAN_POINT('Ctrl Pts',(1.7188807715095,-1.,-1.34634568653586));
#23249=CARTESIAN_POINT('Ctrl Pts',(1.72527410681298,-1.,-1.34716554820013));
#23250=CARTESIAN_POINT('Ctrl Pts',(1.73040149654497,-1.,-1.3477930915247));
#23251=CARTESIAN_POINT('Ctrl Pts',(1.73425417886254,-1.,-1.34824783113158));
#23252=CARTESIAN_POINT('Ctrl Pts',(1.73682580585819,-1.,-1.34854391898145));
#23253=CARTESIAN_POINT('Ctrl Pts',(1.73811241238545,-1.,-1.34869019493419));
#23254=CARTESIAN_POINT('',(1.81978687191668,-1.,-1.23627494547115));
#23255=CARTESIAN_POINT('',(1.73811241238545,-1.,-1.34869019493419));
#23256=CARTESIAN_POINT('',(1.5055822144029,-1.,-0.892032620296855));
#23257=CARTESIAN_POINT('Ctrl Pts',(1.81978687191668,-1.,-1.23627494547115));
#23258=CARTESIAN_POINT('Ctrl Pts',(1.81925017193531,-1.,-1.23509651170384));
#23259=CARTESIAN_POINT('Ctrl Pts',(1.81817389920914,-1.,-1.23274224526804));
#23260=CARTESIAN_POINT('Ctrl Pts',(1.81655087183054,-1.,-1.22921864890975));
#23261=CARTESIAN_POINT('Ctrl Pts',(1.81436959209778,-1.,-1.22453613304507));
#23262=CARTESIAN_POINT('Ctrl Pts',(1.81161420806172,-1.,-1.2187090610323));
#23263=CARTESIAN_POINT('Ctrl Pts',(1.80882996916931,-1.,-1.2129081570818));
#23264=CARTESIAN_POINT('Ctrl Pts',(1.80601678480772,-1.,-1.20713356605519));
#23265=CARTESIAN_POINT('Ctrl Pts',(1.8031745483882,-1.,-1.2013854893912));
#23266=CARTESIAN_POINT('Ctrl Pts',(1.80030314370121,-1.,-1.19566418930405));
#23267=CARTESIAN_POINT('Ctrl Pts',(1.79740245923649,-1.,-1.1899699793456));
#23268=CARTESIAN_POINT('Ctrl Pts',(1.79447240321572,-1.,-1.18430321697471));
#23269=CARTESIAN_POINT('Ctrl Pts',(1.79151291552646,-1.,-1.17866429440781));
#23270=CARTESIAN_POINT('Ctrl Pts',(1.78852398877523,-1.,-1.17305363177265));
#23271=CARTESIAN_POINT('Ctrl Pts',(1.78550566040349,-1.,-1.16747166312239));
#23272=CARTESIAN_POINT('Ctrl Pts',(1.78245795880949,-1.,-1.16191881298458));
#23273=CARTESIAN_POINT('Ctrl Pts',(1.77938085564261,-1.,-1.15639547194689));
#23274=CARTESIAN_POINT('Ctrl Pts',(1.77627422557034,-1.,-1.15090197841531));
#23275=CARTESIAN_POINT('Ctrl Pts',(1.77313777896234,-1.,-1.14543858226948));
#23276=CARTESIAN_POINT('Ctrl Pts',(1.76997111386806,-1.,-1.14000548337));
#23277=CARTESIAN_POINT('Ctrl Pts',(1.76677384551883,-1.,-1.13460291804635));
#23278=CARTESIAN_POINT('Ctrl Pts',(1.76354571966171,-1.,-1.12923123555076));
#23279=CARTESIAN_POINT('Ctrl Pts',(1.76028671825084,-1.,-1.12389096855078));
#23280=CARTESIAN_POINT('Ctrl Pts',(1.75699720772089,-1.,-1.11858293216752));
#23281=CARTESIAN_POINT('Ctrl Pts',(1.75367772094617,-1.,-1.11330807582542));
#23282=CARTESIAN_POINT('Ctrl Pts',(1.75032866075914,-1.,-1.10806728183003));
#23283=CARTESIAN_POINT('Ctrl Pts',(1.74695004214924,-1.,-1.10286118991144));
#23284=CARTESIAN_POINT('Ctrl Pts',(1.74354119236212,-1.,-1.09768999241229));
#23285=CARTESIAN_POINT('Ctrl Pts',(1.74010053962252,-1.,-1.09255329056496));
#23286=CARTESIAN_POINT('Ctrl Pts',(1.73662628326093,-1.,-1.08745056285429));
#23287=CARTESIAN_POINT('Ctrl Pts',(1.73311705663407,-1.,-1.08238162784749));
#23288=CARTESIAN_POINT('Ctrl Pts',(1.72957248977424,-1.,-1.0773470373727));
#23289=CARTESIAN_POINT('Ctrl Pts',(1.72599406198489,-1.,-1.07234866990252));
#23290=CARTESIAN_POINT('Ctrl Pts',(1.72238500928456,-1.,-1.06738966975463));
#23291=CARTESIAN_POINT('Ctrl Pts',(1.71874858456908,-1.,-1.0624732468065));
#23292=CARTESIAN_POINT('Ctrl Pts',(1.71508654427022,-1.,-1.05760163192481));
#23293=CARTESIAN_POINT('Ctrl Pts',(1.71139783543986,-1.,-1.05277517202854));
#23294=CARTESIAN_POINT('Ctrl Pts',(1.70767646263641,-1.,-1.0479908540499));
#23295=CARTESIAN_POINT('Ctrl Pts',(1.70391338707969,-1.,-1.04324363334546));
#23296=CARTESIAN_POINT('Ctrl Pts',(1.70010052930951,-1.,-1.03852922490782));
#23297=CARTESIAN_POINT('Ctrl Pts',(1.69623414782769,-1.,-1.03384646003587));
#23298=CARTESIAN_POINT('Ctrl Pts',(1.69231840863471,-1.,-1.02919977579155));
#23299=CARTESIAN_POINT('Ctrl Pts',(1.68836910178475,-1.,-1.02460180535272));
#23300=CARTESIAN_POINT('Ctrl Pts',(1.68440578021739,-1.,-1.02006795074222));
#23301=CARTESIAN_POINT('Ctrl Pts',(1.6804428989482,-1.,-1.01561026162787));
#23302=CARTESIAN_POINT('Ctrl Pts',(1.67648246776457,-1.,-1.01123236493507));
#23303=CARTESIAN_POINT('Ctrl Pts',(1.67250335383248,-1.,-1.00692206696387));
#23304=CARTESIAN_POINT('Ctrl Pts',(1.66846059277231,-1.,-1.00265091003682));
#23305=CARTESIAN_POINT('Ctrl Pts',(1.66430758030304,-1.,-0.998389654952317));
#23306=CARTESIAN_POINT('Ctrl Pts',(1.66001553809916,-1.,-0.994121836661116));
#23307=CARTESIAN_POINT('Ctrl Pts',(1.65559044289746,-1.,-0.98985562785445));
#23308=CARTESIAN_POINT('Ctrl Pts',(1.6511001661277,-1.,-0.985642622921626));
#23309=CARTESIAN_POINT('Ctrl Pts',(1.64665139190834,-1.,-0.981562530940574));
#23310=CARTESIAN_POINT('Ctrl Pts',(1.64233990826831,-1.,-0.977689794120297));
#23311=CARTESIAN_POINT('Ctrl Pts',(1.63820952658157,-1.,-0.974066058287501));
#23312=CARTESIAN_POINT('Ctrl Pts',(1.63420665729609,-1.,-0.970669715996356));
#23313=CARTESIAN_POINT('Ctrl Pts',(1.63013849959083,-1.,-0.967387853228041));
#23314=CARTESIAN_POINT('Ctrl Pts',(1.6257193066974,-1.,-0.964046107037821));
#23315=CARTESIAN_POINT('Ctrl Pts',(1.62061638139929,-1.,-0.960438326099958));
#23316=CARTESIAN_POINT('Ctrl Pts',(1.61449324337233,-1.,-0.956354422921573));
#23317=CARTESIAN_POINT('Ctrl Pts',(1.60706069897794,-1.,-0.951613284361248));
#23318=CARTESIAN_POINT('Ctrl Pts',(1.59810042045408,-1.,-0.946078063325796));
#23319=CARTESIAN_POINT('Ctrl Pts',(1.58744937489796,-1.,-0.939646377909319));
#23320=CARTESIAN_POINT('Ctrl Pts',(1.57499388385561,-1.,-0.932246680128849));
#23321=CARTESIAN_POINT('Ctrl Pts',(1.56065988582509,-1.,-0.923832188966322));
#23322=CARTESIAN_POINT('Ctrl Pts',(1.54440491152807,-1.,-0.91437591904658));
#23323=CARTESIAN_POINT('Ctrl Pts',(1.52984849890434,-1.,-0.905967409640499));
#23324=CARTESIAN_POINT('Ctrl Pts',(1.51805569591479,-1.,-0.89918504749193));
#23325=CARTESIAN_POINT('Ctrl Pts',(1.50980486807181,-1.,-0.894452006967538));
#23326=CARTESIAN_POINT('Ctrl Pts',(1.5055822144029,-1.,-0.892032620296855));
#23327=CARTESIAN_POINT('',(1.60662857109684,-1.,-0.693717979106306));
#23328=CARTESIAN_POINT('Origin',(0.,-1.,0.));
#23329=CARTESIAN_POINT('',(2.0698113262342,-1.,-0.745574324794401));
#23330=CARTESIAN_POINT('Ctrl Pts',(1.60662857109684,-1.,-0.693717979106306));
#23331=CARTESIAN_POINT('Ctrl Pts',(1.61106790957619,-1.,-0.69571209787897));
#23332=CARTESIAN_POINT('Ctrl Pts',(1.61974673471117,-1.,-0.699605146398837));
#23333=CARTESIAN_POINT('Ctrl Pts',(1.6321654166204,-1.,-0.705159151977294));
#23334=CARTESIAN_POINT('Ctrl Pts',(1.64752408828442,-1.,-0.711993139340448));
#23335=CARTESIAN_POINT('Ctrl Pts',(1.66472880551777,-1.,-0.71958543378795));
#23336=CARTESIAN_POINT('Ctrl Pts',(1.67996158451922,-1.,-0.726235967982445));
#23337=CARTESIAN_POINT('Ctrl Pts',(1.69326921972915,-1.,-0.731963238685357));
#23338=CARTESIAN_POINT('Ctrl Pts',(1.70473309004249,-1.,-0.736799665716932));
#23339=CARTESIAN_POINT('Ctrl Pts',(1.71447789751001,-1.,-0.74079516202821));
#23340=CARTESIAN_POINT('Ctrl Pts',(1.72268229916769,-1.,-0.744021445433094));
#23341=CARTESIAN_POINT('Ctrl Pts',(1.72958533647714,-1.,-0.746574710097752));
#23342=CARTESIAN_POINT('Ctrl Pts',(1.7355035168033,-1.,-0.74858246295687));
#23343=CARTESIAN_POINT('Ctrl Pts',(1.74080458267114,-1.,-0.75019343598125));
#23344=CARTESIAN_POINT('Ctrl Pts',(1.74585086852502,-1.,-0.751555614164483));
#23345=CARTESIAN_POINT('Ctrl Pts',(1.75095139468794,-1.,-0.752797683531314));
#23346=CARTESIAN_POINT('Ctrl Pts',(1.75631083600019,-1.,-0.754009254027829));
#23347=CARTESIAN_POINT('Ctrl Pts',(1.76197817240128,-1.,-0.755220979974462));
#23348=CARTESIAN_POINT('Ctrl Pts',(1.76789396002998,-1.,-0.75642189602781));
#23349=CARTESIAN_POINT('Ctrl Pts',(1.77394167108292,-1.,-0.757578264077029));
#23350=CARTESIAN_POINT('Ctrl Pts',(1.77999411220945,-1.,-0.758650626677519));
#23351=CARTESIAN_POINT('Ctrl Pts',(1.78596964884604,-1.,-0.75961440111019));
#23352=CARTESIAN_POINT('Ctrl Pts',(1.7918581561088,-1.,-0.760469555880749));
#23353=CARTESIAN_POINT('Ctrl Pts',(1.79768986997783,-1.,-0.761229695230558));
#23354=CARTESIAN_POINT('Ctrl Pts',(1.80351583877342,-1.,-0.761915336443547));
#23355=CARTESIAN_POINT('Ctrl Pts',(1.80938551463965,-1.,-0.762546129463938));
#23356=CARTESIAN_POINT('Ctrl Pts',(1.8153211840553,-1.,-0.763132003836634));
#23357=CARTESIAN_POINT('Ctrl Pts',(1.82131873145266,-1.,-0.763673465462727));
#23358=CARTESIAN_POINT('Ctrl Pts',(1.82735991200065,-1.,-0.764165902605995));
#23359=CARTESIAN_POINT('Ctrl Pts',(1.83342077227142,-1.,-0.764602549687853));
#23360=CARTESIAN_POINT('Ctrl Pts',(1.83948181064835,-1.,-0.764978057881738));
#23361=CARTESIAN_POINT('Ctrl Pts',(1.84553698875924,-1.,-0.765291664862029));
#23362=CARTESIAN_POINT('Ctrl Pts',(1.85158945130063,-1.,-0.765545710619063));
#23363=CARTESIAN_POINT('Ctrl Pts',(1.85764741390394,-1.,-0.765744212909319));
#23364=CARTESIAN_POINT('Ctrl Pts',(1.86372027063312,-1.,-0.765891519092547));
#23365=CARTESIAN_POINT('Ctrl Pts',(1.86981398314341,-1.,-0.765990708546091));
#23366=CARTESIAN_POINT('Ctrl Pts',(1.87592888967883,-1.,-0.766042837036744));
#23367=CARTESIAN_POINT('Ctrl Pts',(1.88206215302561,-1.,-0.766047794851865));
#23368=CARTESIAN_POINT('Ctrl Pts',(1.88820926433409,-1.,-0.766004837062091));
#23369=CARTESIAN_POINT('Ctrl Pts',(1.89436577771388,-1.,-0.765913193856978));
#23370=CARTESIAN_POINT('Ctrl Pts',(1.90052930393596,-1.,-0.765772772593386));
#23371=CARTESIAN_POINT('Ctrl Pts',(1.90669961402356,-1.,-0.765584196937919));
#23372=CARTESIAN_POINT('Ctrl Pts',(1.91287765805169,-1.,-0.765348465884722));
#23373=CARTESIAN_POINT('Ctrl Pts',(1.91906491634196,-1.,-0.765066729667089));
#23374=CARTESIAN_POINT('Ctrl Pts',(1.92526263537048,-1.,-0.764740025488212));
#23375=CARTESIAN_POINT('Ctrl Pts',(1.93147105496382,-1.,-0.764369010673941));
#23376=CARTESIAN_POINT('Ctrl Pts',(1.93768964875886,-1.,-0.763954049121459));
#23377=CARTESIAN_POINT('Ctrl Pts',(1.9439174661764,-1.,-0.763495333538629));
#23378=CARTESIAN_POINT('Ctrl Pts',(1.95015342590024,-1.,-0.762992990878769));
#23379=CARTESIAN_POINT('Ctrl Pts',(1.95639665309869,-1.,-0.762447203806179));
#23380=CARTESIAN_POINT('Ctrl Pts',(1.96264672744186,-1.,-0.761858300014424));
#23381=CARTESIAN_POINT('Ctrl Pts',(1.96890351582499,-1.,-0.761226690483821));
#23382=CARTESIAN_POINT('Ctrl Pts',(1.97516705321494,-1.,-0.760552825409757));
#23383=CARTESIAN_POINT('Ctrl Pts',(1.98143741418172,-1.,-0.75983714745219));
#23384=CARTESIAN_POINT('Ctrl Pts',(1.98771456680874,-1.,-0.759080037802488));
#23385=CARTESIAN_POINT('Ctrl Pts',(1.99399831098817,-1.,-0.758281796766761));
#23386=CARTESIAN_POINT('Ctrl Pts',(2.00028834739178,-1.,-0.757442676862724));
#23387=CARTESIAN_POINT('Ctrl Pts',(2.0065843158773,-1.,-0.756562904646671));
#23388=CARTESIAN_POINT('Ctrl Pts',(2.01288584328084,-1.,-0.755642704957865));
#23389=CARTESIAN_POINT('Ctrl Pts',(2.01919259405809,-1.,-0.754682330722816));
#23390=CARTESIAN_POINT('Ctrl Pts',(2.02550428623313,-1.,-0.753682061112768));
#23391=CARTESIAN_POINT('Ctrl Pts',(2.03182068456221,-1.,-0.752642180487211));
#23392=CARTESIAN_POINT('Ctrl Pts',(2.03814160092099,-1.,-0.751562963361115));
#23393=CARTESIAN_POINT('Ctrl Pts',(2.04446689147979,-1.,-0.750444657875576));
#23394=CARTESIAN_POINT('Ctrl Pts',(2.05079645592154,-1.,-0.749287468665046));
#23395=CARTESIAN_POINT('Ctrl Pts',(2.05713023031006,-1.,-0.748091554183803));
#23396=CARTESIAN_POINT('Ctrl Pts',(2.06220058927826,-1.,-0.74710393278792));
#23397=CARTESIAN_POINT('Ctrl Pts',(2.06600523016815,-1.,-0.746345871544201));
#23398=CARTESIAN_POINT('Ctrl Pts',(2.06854248895728,-1.,-0.745832791378367));
#23399=CARTESIAN_POINT('Ctrl Pts',(2.0698113262342,-1.,-0.745574324794401));
#23400=CARTESIAN_POINT('',(2.11275013067528,-1.,-0.61342227326009));
#23401=CARTESIAN_POINT('',(2.0698113262342,-1.,-0.745574324794401));
#23402=CARTESIAN_POINT('',(1.7075470150345,-1.,-0.383122945602004));
#23403=CARTESIAN_POINT('Ctrl Pts',(2.11275013067528,-1.,-0.61342227326009));
#23404=CARTESIAN_POINT('Ctrl Pts',(2.11187554259986,-1.,-0.6124673655618));
#23405=CARTESIAN_POINT('Ctrl Pts',(2.11012443807238,-1.,-0.610560911689899));
#23406=CARTESIAN_POINT('Ctrl Pts',(2.1074919961518,-1.,-0.607711315454876));
#23407=CARTESIAN_POINT('Ctrl Pts',(2.10397049886949,-1.,-0.60393203073603));
#23408=CARTESIAN_POINT('Ctrl Pts',(2.0995493086477,-1.,-0.599241616420534));
#23409=CARTESIAN_POINT('Ctrl Pts',(2.0951087622027,-1.,-0.594585006052162));
#23410=CARTESIAN_POINT('Ctrl Pts',(2.09064881812129,-1.,-0.589962365403406));
#23411=CARTESIAN_POINT('Ctrl Pts',(2.08616943727951,-1.,-0.585373918991617));
#23412=CARTESIAN_POINT('Ctrl Pts',(2.08167059018418,-1.,-0.580819952108064));
#23413=CARTESIAN_POINT('Ctrl Pts',(2.07715226767559,-1.,-0.576300797416845));
#23414=CARTESIAN_POINT('Ctrl Pts',(2.07261449292824,-1.,-0.571816823242603));
#23415=CARTESIAN_POINT('Ctrl Pts',(2.06805732997334,-1.,-0.567368421181087));
#23416=CARTESIAN_POINT('Ctrl Pts',(2.06348090160589,-1.,-0.562955993082262));
#23417=CARTESIAN_POINT('Ctrl Pts',(2.05888537756462,-1.,-0.558579940185152));
#23418=CARTESIAN_POINT('Ctrl Pts',(2.05427091604413,-1.,-0.554240657463906));
#23419=CARTESIAN_POINT('Ctrl Pts',(2.04963761077958,-1.,-0.549938525150295));
#23420=CARTESIAN_POINT('Ctrl Pts',(2.04498544714588,-1.,-0.54567390381743));
#23421=CARTESIAN_POINT('Ctrl Pts',(2.04031422690527,-1.,-0.541447120615659));
#23422=CARTESIAN_POINT('Ctrl Pts',(2.03562362954037,-1.,-0.537258489833262));
#23423=CARTESIAN_POINT('Ctrl Pts',(2.03091336214426,-1.,-0.533108355132977));
#23424=CARTESIAN_POINT('Ctrl Pts',(2.0261832908329,-1.,-0.528997127241914));
#23425=CARTESIAN_POINT('Ctrl Pts',(2.02143356304698,-1.,-0.524925318333476));
#23426=CARTESIAN_POINT('Ctrl Pts',(2.01666477917286,-1.,-0.520893590399371));
#23427=CARTESIAN_POINT('Ctrl Pts',(2.01187773939242,-1.,-0.516902681728687));
#23428=CARTESIAN_POINT('Ctrl Pts',(2.00707309946949,-1.,-0.512953306961793));
#23429=CARTESIAN_POINT('Ctrl Pts',(2.00225107134734,-1.,-0.509046069886157));
#23430=CARTESIAN_POINT('Ctrl Pts',(1.99741107463572,-1.,-0.505181361323026));
#23431=CARTESIAN_POINT('Ctrl Pts',(1.99255149126155,-1.,-0.501359287727146));
#23432=CARTESIAN_POINT('Ctrl Pts',(1.98767044752932,-1.,-0.497579909545574));
#23433=CARTESIAN_POINT('Ctrl Pts',(1.98276658761821,-1.,-0.493843476541495));
#23434=CARTESIAN_POINT('Ctrl Pts',(1.97783973019229,-1.,-0.490150627860953));
#23435=CARTESIAN_POINT('Ctrl Pts',(1.97289186263272,-1.,-0.486502692907659));
#23436=CARTESIAN_POINT('Ctrl Pts',(1.96792703422362,-1.,-0.482901662120691));
#23437=CARTESIAN_POINT('Ctrl Pts',(1.96294933055943,-1.,-0.479349583074855));
#23438=CARTESIAN_POINT('Ctrl Pts',(1.95796111148177,-1.,-0.475848034683176));
#23439=CARTESIAN_POINT('Ctrl Pts',(1.95296148278133,-1.,-0.472397672264072));
#23440=CARTESIAN_POINT('Ctrl Pts',(1.94794381136514,-1.,-0.468997482913135));
#23441=CARTESIAN_POINT('Ctrl Pts',(1.9428979419619,-1.,-0.46564546202603));
#23442=CARTESIAN_POINT('Ctrl Pts',(1.93781486640821,-1.,-0.462340031009057));
#23443=CARTESIAN_POINT('Ctrl Pts',(1.93269066517934,-1.,-0.459081234547926));
#23444=CARTESIAN_POINT('Ctrl Pts',(1.92753067150476,-1.,-0.455872005174371));
#23445=CARTESIAN_POINT('Ctrl Pts',(1.92235380648502,-1.,-0.452719478359433));
#23446=CARTESIAN_POINT('Ctrl Pts',(1.91718342555755,-1.,-0.449632260106662));
#23447=CARTESIAN_POINT('Ctrl Pts',(1.9120369998112,-1.,-0.446617343485711));
#23448=CARTESIAN_POINT('Ctrl Pts',(1.90691756144898,-1.,-0.443677556849151));
#23449=CARTESIAN_POINT('Ctrl Pts',(1.90180124389086,-1.,-0.440807833704038));
#23450=CARTESIAN_POINT('Ctrl Pts',(1.89663648956466,-1.,-0.437995003948244));
#23451=CARTESIAN_POINT('Ctrl Pts',(1.89136993975504,-1.,-0.435225660963383));
#23452=CARTESIAN_POINT('Ctrl Pts',(1.88596913666793,-1.,-0.432493038548748));
#23453=CARTESIAN_POINT('Ctrl Pts',(1.88044229001832,-1.,-0.429803062482345));
#23454=CARTESIAN_POINT('Ctrl Pts',(1.87486989291484,-1.,-0.427183828519102));
#23455=CARTESIAN_POINT('Ctrl Pts',(1.86937803944323,-1.,-0.424678177291359));
#23456=CARTESIAN_POINT('Ctrl Pts',(1.86408083334028,-1.,-0.422327307418275));
#23457=CARTESIAN_POINT('Ctrl Pts',(1.85903281096686,-1.,-0.42015728797562));
#23458=CARTESIAN_POINT('Ctrl Pts',(1.85417632856234,-1.,-0.418164129143534));
#23459=CARTESIAN_POINT('Ctrl Pts',(1.84929312929882,-1.,-0.416300022038864));
#23460=CARTESIAN_POINT('Ctrl Pts',(1.8440575707371,-1.,-0.41448743825434));
#23461=CARTESIAN_POINT('Ctrl Pts',(1.83808953475839,-1.,-0.412633125322162));
#23462=CARTESIAN_POINT('Ctrl Pts',(1.83100408895216,-1.,-0.410641256301675));
#23463=CARTESIAN_POINT('Ctrl Pts',(1.8224702267854,-1.,-0.408428948108534));
#23464=CARTESIAN_POINT('Ctrl Pts',(1.81223801813988,-1.,-0.405933518411838));
#23465=CARTESIAN_POINT('Ctrl Pts',(1.80012077176221,-1.,-0.403107976170441));
#23466=CARTESIAN_POINT('Ctrl Pts',(1.78598826347533,-1.,-0.399919403783081));
#23467=CARTESIAN_POINT('Ctrl Pts',(1.7697556004756,-1.,-0.39634619612042));
#23468=CARTESIAN_POINT('Ctrl Pts',(1.75137405313962,-1.,-0.392375812294307));
#23469=CARTESIAN_POINT('Ctrl Pts',(1.7349317097561,-1.,-0.388877023509192));
#23470=CARTESIAN_POINT('Ctrl Pts',(1.72162022246158,-1.,-0.38607079032701));
#23471=CARTESIAN_POINT('Ctrl Pts',(1.71231062891958,-1.,-0.384119047315542));
#23472=CARTESIAN_POINT('Ctrl Pts',(1.7075470150345,-1.,-0.383122945602004));
#23473=CARTESIAN_POINT('',(1.74236521665491,-1.,-0.163289472382896));
#23474=CARTESIAN_POINT('Origin',(0.,-1.,0.));
#23475=CARTESIAN_POINT('',(2.19890268624765,-1.,-0.0694764450219582));
#23476=CARTESIAN_POINT('Ctrl Pts',(1.74236521665491,-1.,-0.163289472382896));
#23477=CARTESIAN_POINT('Ctrl Pts',(1.7472034950333,-1.,-0.163814161002002));
#23478=CARTESIAN_POINT('Ctrl Pts',(1.75666056638427,-1.,-0.164834765707159));
#23479=CARTESIAN_POINT('Ctrl Pts',(1.77018771684844,-1.,-0.1662793551464));
#23480=CARTESIAN_POINT('Ctrl Pts',(1.7869064998507,-1.,-0.168032772805197));
#23481=CARTESIAN_POINT('Ctrl Pts',(1.80561530629706,-1.,-0.169936923904608));
#23482=CARTESIAN_POINT('Ctrl Pts',(1.82215766811545,-1.,-0.171554770204119));
#23483=CARTESIAN_POINT('Ctrl Pts',(1.83658380527692,-1.,-0.1728894428919));
#23484=CARTESIAN_POINT('Ctrl Pts',(1.8489811319852,-1.,-0.173946627587732));
#23485=CARTESIAN_POINT('Ctrl Pts',(1.85948367088837,-1.,-0.17473525927603));
#23486=CARTESIAN_POINT('Ctrl Pts',(1.86828349694799,-1.,-0.175268337590758));
#23487=CARTESIAN_POINT('Ctrl Pts',(1.87563767773588,-1.,-0.175563480746485));
#23488=CARTESIAN_POINT('Ctrl Pts',(1.88188663145367,-1.,-0.175644148889699));
#23489=CARTESIAN_POINT('Ctrl Pts',(1.88742606273259,-1.,-0.175538155840648));
#23490=CARTESIAN_POINT('Ctrl Pts',(1.892646301985,-1.,-0.175274276190844));
#23491=CARTESIAN_POINT('Ctrl Pts',(1.89788101117132,-1.,-0.174879405091263));
#23492=CARTESIAN_POINT('Ctrl Pts',(1.90335253862834,-1.,-0.174375518661085));
#23493=CARTESIAN_POINT('Ctrl Pts',(1.90911693975267,-1.,-0.173776635257817));
#23494=CARTESIAN_POINT('Ctrl Pts',(1.91511429159527,-1.,-0.173090695383496));
#23495=CARTESIAN_POINT('Ctrl Pts',(1.9212233439798,-1.,-0.172321621259514));
#23496=CARTESIAN_POINT('Ctrl Pts',(1.92731093582036,-1.,-0.171471191532988));
#23497=CARTESIAN_POINT('Ctrl Pts',(1.93329183155539,-1.,-0.170541253116202));
#23498=CARTESIAN_POINT('Ctrl Pts',(1.93915639211581,-1.,-0.169534904817491));
#23499=CARTESIAN_POINT('Ctrl Pts',(1.94493757756931,-1.,-0.168455741607556));
#23500=CARTESIAN_POINT('Ctrl Pts',(1.95069027794294,-1.,-0.167307501784476));
#23501=CARTESIAN_POINT('Ctrl Pts',(1.9564675971873,-1.,-0.166093592002813));
#23502=CARTESIAN_POINT('Ctrl Pts',(1.96229379940136,-1.,-0.164816568920269));
#23503=CARTESIAN_POINT('Ctrl Pts',(1.96816512677967,-1.,-0.163478185457734));
#23504=CARTESIAN_POINT('Ctrl Pts',(1.97406280235188,-1.,-0.162079693556289));
#23505=CARTESIAN_POINT('Ctrl Pts',(1.97996195437559,-1.,-0.160622060784611));
#23506=CARTESIAN_POINT('Ctrl Pts',(1.98584238283292,-1.,-0.159106226437299));
#23507=CARTESIAN_POINT('Ctrl Pts',(1.99169810931908,-1.,-0.157533331459227));
#23508=CARTESIAN_POINT('Ctrl Pts',(1.99753284771497,-1.,-0.155904629548784));
#23509=CARTESIAN_POINT('Ctrl Pts',(2.00335565310543,-1.,-0.154221403049722));
#23510=CARTESIAN_POINT('Ctrl Pts',(2.00917680318424,-1.,-0.15248488362145));
#23511=CARTESIAN_POINT('Ctrl Pts',(2.01500291940238,-1.,-0.150696157673078));
#23512=CARTESIAN_POINT('Ctrl Pts',(2.02083464969894,-1.,-0.148856124775337));
#23513=CARTESIAN_POINT('Ctrl Pts',(2.02666926182017,-1.,-0.146965557332583));
#23514=CARTESIAN_POINT('Ctrl Pts',(2.03250223739942,-1.,-0.145025140186058));
#23515=CARTESIAN_POINT('Ctrl Pts',(2.03832911025912,-1.,-0.143035515058209));
#23516=CARTESIAN_POINT('Ctrl Pts',(2.04414757947916,-1.,-0.140997332152546));
#23517=CARTESIAN_POINT('Ctrl Pts',(2.04995762001328,-1.,-0.138911255368966));
#23518=CARTESIAN_POINT('Ctrl Pts',(2.05576044414264,-1.,-0.136777941218044));
#23519=CARTESIAN_POINT('Ctrl Pts',(2.06155781517842,-1.,-0.134598026192106));
#23520=CARTESIAN_POINT('Ctrl Pts',(2.06735123910326,-1.,-0.132372111547711));
#23521=CARTESIAN_POINT('Ctrl Pts',(2.07314114713063,-1.,-0.130100748328404));
#23522=CARTESIAN_POINT('Ctrl Pts',(2.07892715110987,-1.,-0.12778444527612));
#23523=CARTESIAN_POINT('Ctrl Pts',(2.08470840653643,-1.,-0.125423679412062));
#23524=CARTESIAN_POINT('Ctrl Pts',(2.09048392424825,-1.,-0.123018905621083));
#23525=CARTESIAN_POINT('Ctrl Pts',(2.0962529286773,-1.,-0.120570567965122));
#23526=CARTESIAN_POINT('Ctrl Pts',(2.102015121329,-1.,-0.118079107988356));
#23527=CARTESIAN_POINT('Ctrl Pts',(2.10777050261309,-1.,-0.115544957687927));
#23528=CARTESIAN_POINT('Ctrl Pts',(2.11351924490306,-1.,-0.112968534419737));
#23529=CARTESIAN_POINT('Ctrl Pts',(2.11926155590865,-1.,-0.110350236135025));
#23530=CARTESIAN_POINT('Ctrl Pts',(2.12499752307,-1.,-0.10769043523109));
#23531=CARTESIAN_POINT('Ctrl Pts',(2.13072704887293,-1.,-0.10498947915274));
#23532=CARTESIAN_POINT('Ctrl Pts',(2.13644992667165,-1.,-0.102247700556101));
#23533=CARTESIAN_POINT('Ctrl Pts',(2.14216588396025,-1.,-0.0994654261990917));
#23534=CARTESIAN_POINT('Ctrl Pts',(2.14787463531795,-1.,-0.096642985230546));
#23535=CARTESIAN_POINT('Ctrl Pts',(2.1535759397817,-1.,-0.0937807218867645));
#23536=CARTESIAN_POINT('Ctrl Pts',(2.15926961544516,-1.,-0.0908789888107267));
#23537=CARTESIAN_POINT('Ctrl Pts',(2.16495552645014,-1.,-0.0879381291386924));
#23538=CARTESIAN_POINT('Ctrl Pts',(2.17063357870952,-1.,-0.0849584620835374));
#23539=CARTESIAN_POINT('Ctrl Pts',(2.176303712113,-1.,-0.0819402680872767));
#23540=CARTESIAN_POINT('Ctrl Pts',(2.18196589448887,-1.,-0.0788837727685244));
#23541=CARTESIAN_POINT('Ctrl Pts',(2.1876201139953,-1.,-0.0757891465836149));
#23542=CARTESIAN_POINT('Ctrl Pts',(2.19213712013662,-1.,-0.0732830357306726));
#23543=CARTESIAN_POINT('Ctrl Pts',(2.19552129484002,-1.,-0.0713863779526155));
#23544=CARTESIAN_POINT('Ctrl Pts',(2.19777582085423,-1.,-0.0701143536325491));
#23545=CARTESIAN_POINT('Ctrl Pts',(2.19890268624765,-1.,-0.0694764450219582));
#23546=CARTESIAN_POINT('',(2.19890268624765,-1.,0.0694764450219582));
#23547=CARTESIAN_POINT('',(2.19890268624765,-1.,-0.0694764450219582));
#23548=CARTESIAN_POINT('',(1.74236521665491,-1.,0.163289472382896));
#23549=CARTESIAN_POINT('Ctrl Pts',(2.19890268624765,-1.,0.0694764450219582));
#23550=CARTESIAN_POINT('Ctrl Pts',(2.19777582085261,-1.,0.0701143536324925));
#23551=CARTESIAN_POINT('Ctrl Pts',(2.19552129483562,-1.,0.0713863779524626));
#23552=CARTESIAN_POINT('Ctrl Pts',(2.19213712012956,-1.,0.0732830357304275));
#23553=CARTESIAN_POINT('Ctrl Pts',(2.1876201139874,-1.,0.075789146583341));
#23554=CARTESIAN_POINT('Ctrl Pts',(2.18196589448304,-1.,0.0788837727683226));
#23555=CARTESIAN_POINT('Ctrl Pts',(2.1763037121106,-1.,0.0819402680871938));
#23556=CARTESIAN_POINT('Ctrl Pts',(2.17063357871031,-1.,0.0849584620835642));
#23557=CARTESIAN_POINT('Ctrl Pts',(2.16495552645275,-1.,0.0879381291387821));
#23558=CARTESIAN_POINT('Ctrl Pts',(2.15926961544808,-1.,0.0908789888108265));
#23559=CARTESIAN_POINT('Ctrl Pts',(2.15357593978377,-1.,0.0937807218868344));
#23560=CARTESIAN_POINT('Ctrl Pts',(2.14787463531864,-1.,0.0966429852305688));
#23561=CARTESIAN_POINT('Ctrl Pts',(2.14216588395974,-1.,0.0994654261990741));
#23562=CARTESIAN_POINT('Ctrl Pts',(2.13644992667052,-1.,0.102247700556063));
#23563=CARTESIAN_POINT('Ctrl Pts',(2.1307270488718,-1.,0.104989479152703));
#23564=CARTESIAN_POINT('Ctrl Pts',(2.12499752306927,-1.,0.107690435231068));
#23565=CARTESIAN_POINT('Ctrl Pts',(2.11926155590849,-1.,0.11035023613502));
#23566=CARTESIAN_POINT('Ctrl Pts',(2.11351924490335,-1.,0.112968534419746));
#23567=CARTESIAN_POINT('Ctrl Pts',(2.10777050261359,-1.,0.11554495768794));
#23568=CARTESIAN_POINT('Ctrl Pts',(2.10201512132945,-1.,0.118079107988368));
#23569=CARTESIAN_POINT('Ctrl Pts',(2.09625292867756,-1.,0.120570567965129));
#23570=CARTESIAN_POINT('Ctrl Pts',(2.09048392424826,-1.,0.123018905621083));
#23571=CARTESIAN_POINT('Ctrl Pts',(2.08470840653628,-1.,0.125423679412058));
#23572=CARTESIAN_POINT('Ctrl Pts',(2.07892715110967,-1.,0.127784445276116));
#23573=CARTESIAN_POINT('Ctrl Pts',(2.07314114713047,-1.,0.1301007483284));
#23574=CARTESIAN_POINT('Ctrl Pts',(2.06735123910319,-1.,0.132372111547709));
#23575=CARTESIAN_POINT('Ctrl Pts',(2.06155781517844,-1.,0.134598026192107));
#23576=CARTESIAN_POINT('Ctrl Pts',(2.0557604441427,-1.,0.136777941218044));
#23577=CARTESIAN_POINT('Ctrl Pts',(2.04995762001333,-1.,0.138911255368966));
#23578=CARTESIAN_POINT('Ctrl Pts',(2.04414757947919,-1.,0.140997332152545));
#23579=CARTESIAN_POINT('Ctrl Pts',(2.03832911025913,-1.,0.143035515058208));
#23580=CARTESIAN_POINT('Ctrl Pts',(2.03250223739941,-1.,0.145025140186058));
#23581=CARTESIAN_POINT('Ctrl Pts',(2.02666926182017,-1.,0.146965557332586));
#23582=CARTESIAN_POINT('Ctrl Pts',(2.02083464969897,-1.,0.148856124775342));
#23583=CARTESIAN_POINT('Ctrl Pts',(2.01500291940243,-1.,0.150696157673084));
#23584=CARTESIAN_POINT('Ctrl Pts',(2.00917680318426,-1.,0.152484883621452));
#23585=CARTESIAN_POINT('Ctrl Pts',(2.00335565310539,-1.,0.154221403049719));
#23586=CARTESIAN_POINT('Ctrl Pts',(1.99753284771487,-1.,0.155904629548774));
#23587=CARTESIAN_POINT('Ctrl Pts',(1.99169810931893,-1.,0.157533331459215));
#23588=CARTESIAN_POINT('Ctrl Pts',(1.98584238283279,-1.,0.159106226437288));
#23589=CARTESIAN_POINT('Ctrl Pts',(1.97996195437557,-1.,0.16062206078461));
#23590=CARTESIAN_POINT('Ctrl Pts',(1.97406280235204,-1.,0.162079693556302));
#23591=CARTESIAN_POINT('Ctrl Pts',(1.96816512678,-1.,0.16347818545776));
#23592=CARTESIAN_POINT('Ctrl Pts',(1.96229379940174,-1.,0.1648165689203));
#23593=CARTESIAN_POINT('Ctrl Pts',(1.95646759718755,-1.,0.166093592002832));
#23594=CARTESIAN_POINT('Ctrl Pts',(1.95069027794286,-1.,0.167307501784469));
#23595=CARTESIAN_POINT('Ctrl Pts',(1.94493757756879,-1.,0.168455741607515));
#23596=CARTESIAN_POINT('Ctrl Pts',(1.93915639211497,-1.,0.169534904817425));
#23597=CARTESIAN_POINT('Ctrl Pts',(1.93329183155455,-1.,0.170541253116136));
#23598=CARTESIAN_POINT('Ctrl Pts',(1.92731093582,-1.,0.17147119153296));
#23599=CARTESIAN_POINT('Ctrl Pts',(1.92122334398034,-1.,0.172321621259556));
#23600=CARTESIAN_POINT('Ctrl Pts',(1.91511429159681,-1.,0.173090695383619));
#23601=CARTESIAN_POINT('Ctrl Pts',(1.90911693975475,-1.,0.173776635257983));
#23602=CARTESIAN_POINT('Ctrl Pts',(1.90335253863003,-1.,0.174375518661222));
#23603=CARTESIAN_POINT('Ctrl Pts',(1.89788101117148,-1.,0.174879405091277));
#23604=CARTESIAN_POINT('Ctrl Pts',(1.89264630198279,-1.,0.175274276190664));
#23605=CARTESIAN_POINT('Ctrl Pts',(1.88742606272818,-1.,0.175538155840286));
#23606=CARTESIAN_POINT('Ctrl Pts',(1.88188663144846,-1.,0.175644148889271));
#23607=CARTESIAN_POINT('Ctrl Pts',(1.87563767773249,-1.,0.175563480746205));
#23608=CARTESIAN_POINT('Ctrl Pts',(1.86828349694972,-1.,0.1752683375909));
#23609=CARTESIAN_POINT('Ctrl Pts',(1.85948367089838,-1.,0.174735259276856));
#23610=CARTESIAN_POINT('Ctrl Pts',(1.84898113200543,-1.,0.173946627589401));
#23611=CARTESIAN_POINT('Ctrl Pts',(1.83658380530747,-1.,0.17288944289442));
#23612=CARTESIAN_POINT('Ctrl Pts',(1.82215766815414,-1.,0.171554770207306));
#23613=CARTESIAN_POINT('Ctrl Pts',(1.80561530633924,-1.,0.169936923908078));
#23614=CARTESIAN_POINT('Ctrl Pts',(1.78690649988931,-1.,0.16803277280837));
#23615=CARTESIAN_POINT('Ctrl Pts',(1.77018771687692,-1.,0.166279355148738));
#23616=CARTESIAN_POINT('Ctrl Pts',(1.75666056640041,-1.,0.164834765708484));
#23617=CARTESIAN_POINT('Ctrl Pts',(1.74720349503904,-1.,0.163814161002474));
#23618=CARTESIAN_POINT('Ctrl Pts',(1.74236521665491,-1.,0.163289472382896));
#23619=CARTESIAN_POINT('',(1.7075470150345,-1.,0.383122945602004));
#23620=CARTESIAN_POINT('Origin',(0.,-1.,0.));
#23621=CARTESIAN_POINT('',(2.11275013067528,-1.,0.613422273260091));
#23622=CARTESIAN_POINT('Ctrl Pts',(1.7075470150345,-1.,0.383122945602004));
#23623=CARTESIAN_POINT('Ctrl Pts',(1.71231062891398,-1.,0.384119047314215));
#23624=CARTESIAN_POINT('Ctrl Pts',(1.72162022244582,-1.,0.386070790323281));
#23625=CARTESIAN_POINT('Ctrl Pts',(1.73493170972829,-1.,0.388877023502615));
#23626=CARTESIAN_POINT('Ctrl Pts',(1.75137405310193,-1.,0.392375812285396));
#23627=CARTESIAN_POINT('Ctrl Pts',(1.76975560043442,-1.,0.396346196110688));
#23628=CARTESIAN_POINT('Ctrl Pts',(1.78598826343754,-1.,0.399919403774156));
#23629=CARTESIAN_POINT('Ctrl Pts',(1.80012077173238,-1.,0.403107976163396));
#23630=CARTESIAN_POINT('Ctrl Pts',(1.81223801812013,-1.,0.405933518407176));
#23631=CARTESIAN_POINT('Ctrl Pts',(1.82247022677562,-1.,0.408428948106228));
#23632=CARTESIAN_POINT('Ctrl Pts',(1.83100408895047,-1.,0.410641256301276));
#23633=CARTESIAN_POINT('Ctrl Pts',(1.8380895347617,-1.,0.412633125322945));
#23634=CARTESIAN_POINT('Ctrl Pts',(1.84405757074218,-1.,0.414487438255542));
#23635=CARTESIAN_POINT('Ctrl Pts',(1.84929312930314,-1.,0.416300022039885));
#23636=CARTESIAN_POINT('Ctrl Pts',(1.8541763285645,-1.,0.418164129144046));
#23637=CARTESIAN_POINT('Ctrl Pts',(1.8590328109667,-1.,0.420157287975583));
#23638=CARTESIAN_POINT('Ctrl Pts',(1.86408083333863,-1.,0.422327307417885));
#23639=CARTESIAN_POINT('Ctrl Pts',(1.8693780394412,-1.,0.424678177290876));
#23640=CARTESIAN_POINT('Ctrl Pts',(1.87486989291333,-1.,0.427183828518743));
#23641=CARTESIAN_POINT('Ctrl Pts',(1.88044229001778,-1.,0.429803062482217));
#23642=CARTESIAN_POINT('Ctrl Pts',(1.88596913666828,-1.,0.432493038548833));
#23643=CARTESIAN_POINT('Ctrl Pts',(1.89136993975585,-1.,0.43522566096358));
#23644=CARTESIAN_POINT('Ctrl Pts',(1.89663648956549,-1.,0.437995003948443));
#23645=CARTESIAN_POINT('Ctrl Pts',(1.90180124389137,-1.,0.440807833704161));
#23646=CARTESIAN_POINT('Ctrl Pts',(1.90691756144906,-1.,0.443677556849171));
#23647=CARTESIAN_POINT('Ctrl Pts',(1.91203699981095,-1.,0.446617343485651));
#23648=CARTESIAN_POINT('Ctrl Pts',(1.91718342555717,-1.,0.449632260106572));
#23649=CARTESIAN_POINT('Ctrl Pts',(1.9223538064847,-1.,0.452719478359356));
#23650=CARTESIAN_POINT('Ctrl Pts',(1.92753067150461,-1.,0.455872005174336));
#23651=CARTESIAN_POINT('Ctrl Pts',(1.93269066517936,-1.,0.459081234547932));
#23652=CARTESIAN_POINT('Ctrl Pts',(1.93781486640834,-1.,0.462340031009087));
#23653=CARTESIAN_POINT('Ctrl Pts',(1.94289794196205,-1.,0.465645462026065));
#23654=CARTESIAN_POINT('Ctrl Pts',(1.94794381136524,-1.,0.468997482913158));
#23655=CARTESIAN_POINT('Ctrl Pts',(1.95296148278136,-1.,0.47239767226408));
#23656=CARTESIAN_POINT('Ctrl Pts',(1.95796111148175,-1.,0.475848034683172));
#23657=CARTESIAN_POINT('Ctrl Pts',(1.96294933055938,-1.,0.479349583074846));
#23658=CARTESIAN_POINT('Ctrl Pts',(1.96792703422358,-1.,0.482901662120687));
#23659=CARTESIAN_POINT('Ctrl Pts',(1.97289186263272,-1.,0.486502692907661));
#23660=CARTESIAN_POINT('Ctrl Pts',(1.97783973019229,-1.,0.490150627860955));
#23661=CARTESIAN_POINT('Ctrl Pts',(1.9827665876182,-1.,0.493843476541493));
#23662=CARTESIAN_POINT('Ctrl Pts',(1.98767044752929,-1.,0.497579909545564));
#23663=CARTESIAN_POINT('Ctrl Pts',(1.9925514912615,-1.,0.501359287727129));
#23664=CARTESIAN_POINT('Ctrl Pts',(1.99741107463567,-1.,0.505181361323011));
#23665=CARTESIAN_POINT('Ctrl Pts',(2.00225107134733,-1.,0.509046069886152));
#23666=CARTESIAN_POINT('Ctrl Pts',(2.00707309946955,-1.,0.512953306961814));
#23667=CARTESIAN_POINT('Ctrl Pts',(2.01187773939257,-1.,0.516902681728733));
#23668=CARTESIAN_POINT('Ctrl Pts',(2.01666477917305,-1.,0.520893590399429));
#23669=CARTESIAN_POINT('Ctrl Pts',(2.02143356304712,-1.,0.524925318333519));
#23670=CARTESIAN_POINT('Ctrl Pts',(2.02618329083289,-1.,0.528997127241911));
#23671=CARTESIAN_POINT('Ctrl Pts',(2.03091336214401,-1.,0.533108355132905));
#23672=CARTESIAN_POINT('Ctrl Pts',(2.03562362953993,-1.,0.537258489833135));
#23673=CARTESIAN_POINT('Ctrl Pts',(2.0403142269048,-1.,0.54144712061552));
#23674=CARTESIAN_POINT('Ctrl Pts',(2.0449854471456,-1.,0.545673903817349));
#23675=CARTESIAN_POINT('Ctrl Pts',(2.04963761077974,-1.,0.549938525150342));
#23676=CARTESIAN_POINT('Ctrl Pts',(2.05427091604482,-1.,0.55424065746411));
#23677=CARTESIAN_POINT('Ctrl Pts',(2.05888537756571,-1.,0.558579940185468));
#23678=CARTESIAN_POINT('Ctrl Pts',(2.06348090160697,-1.,0.562955993082574));
#23679=CARTESIAN_POINT('Ctrl Pts',(2.06805732997383,-1.,0.56736842118123));
#23680=CARTESIAN_POINT('Ctrl Pts',(2.07261449292757,-1.,0.571816823242411));
#23681=CARTESIAN_POINT('Ctrl Pts',(2.07715226767361,-1.,0.576300797416275));
#23682=CARTESIAN_POINT('Ctrl Pts',(2.08167059018138,-1.,0.580819952107257));
#23683=CARTESIAN_POINT('Ctrl Pts',(2.086169437277,-1.,0.585373918990895));
#23684=CARTESIAN_POINT('Ctrl Pts',(2.09064881812053,-1.,0.58996236540319));
#23685=CARTESIAN_POINT('Ctrl Pts',(2.09510876220501,-1.,0.594585006052824));
#23686=CARTESIAN_POINT('Ctrl Pts',(2.09954930865331,-1.,0.599241616422144));
#23687=CARTESIAN_POINT('Ctrl Pts',(2.10397049887709,-1.,0.603932030738212));
#23688=CARTESIAN_POINT('Ctrl Pts',(2.10749199615859,-1.,0.607711315456826));
#23689=CARTESIAN_POINT('Ctrl Pts',(2.11012443807661,-1.,0.610560911691114));
#23690=CARTESIAN_POINT('Ctrl Pts',(2.11187554260142,-1.,0.61246736556225));
#23691=CARTESIAN_POINT('Ctrl Pts',(2.11275013067528,-1.,0.613422273260091));
#23692=CARTESIAN_POINT('',(2.0698113262342,-1.,0.745574324794401));
#23693=CARTESIAN_POINT('',(2.11275013067528,-1.,0.613422273260091));
#23694=CARTESIAN_POINT('Ctrl Pts',(2.0698113262342,-1.,0.745574324794401));
#23695=CARTESIAN_POINT('Ctrl Pts',(2.06854248895575,-1.,0.74583279137781));
#23696=CARTESIAN_POINT('Ctrl Pts',(2.06600523016401,-1.,0.746345871542696));
#23697=CARTESIAN_POINT('Ctrl Pts',(2.06220058927162,-1.,0.747103932785504));
#23698=CARTESIAN_POINT('Ctrl Pts',(2.05713023030263,-1.,0.748091554181101));
#23699=CARTESIAN_POINT('Ctrl Pts',(2.05079645591606,-1.,0.749287468663053));
#23700=CARTESIAN_POINT('Ctrl Pts',(2.04446689147754,-1.,0.750444657874758));
#23701=CARTESIAN_POINT('Ctrl Pts',(2.03814160092173,-1.,0.751562963361384));
#23702=CARTESIAN_POINT('Ctrl Pts',(2.03182068456467,-1.,0.752642180488104));
#23703=CARTESIAN_POINT('Ctrl Pts',(2.02550428623587,-1.,0.753682061113766));
#23704=CARTESIAN_POINT('Ctrl Pts',(2.01919259406003,-1.,0.75468233072352));
#23705=CARTESIAN_POINT('Ctrl Pts',(2.01288584328149,-1.,0.755642704958101));
#23706=CARTESIAN_POINT('Ctrl Pts',(2.00658431587682,-1.,0.756562904646496));
#23707=CARTESIAN_POINT('Ctrl Pts',(2.00028834739072,-1.,0.757442676862342));
#23708=CARTESIAN_POINT('Ctrl Pts',(1.9939983109871,-1.,0.758281796766377));
#23709=CARTESIAN_POINT('Ctrl Pts',(1.98771456680806,-1.,0.759080037802243));
#23710=CARTESIAN_POINT('Ctrl Pts',(1.98143741418156,-1.,0.759837147452135));
#23711=CARTESIAN_POINT('Ctrl Pts',(1.97516705321521,-1.,0.760552825409856));
#23712=CARTESIAN_POINT('Ctrl Pts',(1.96890351582545,-1.,0.761226690483986));
#23713=CARTESIAN_POINT('Ctrl Pts',(1.96264672744229,-1.,0.761858300014575));
#23714=CARTESIAN_POINT('Ctrl Pts',(1.95639665309893,-1.,0.762447203806264));
#23715=CARTESIAN_POINT('Ctrl Pts',(1.95015342590025,-1.,0.762992990878774));
#23716=CARTESIAN_POINT('Ctrl Pts',(1.94391746617626,-1.,0.763495333538581));
#23717=CARTESIAN_POINT('Ctrl Pts',(1.93768964875867,-1.,0.763954049121394));
#23718=CARTESIAN_POINT('Ctrl Pts',(1.93147105496367,-1.,0.76436901067389));
#23719=CARTESIAN_POINT('Ctrl Pts',(1.92526263537041,-1.,0.764740025488189));
#23720=CARTESIAN_POINT('Ctrl Pts',(1.91906491634197,-1.,0.765066729667095));
#23721=CARTESIAN_POINT('Ctrl Pts',(1.91287765805174,-1.,0.765348465884739));
#23722=CARTESIAN_POINT('Ctrl Pts',(1.90669961402362,-1.,0.765584196937937));
#23723=CARTESIAN_POINT('Ctrl Pts',(1.90052930393599,-1.,0.765772772593395));
#23724=CARTESIAN_POINT('Ctrl Pts',(1.89436577771389,-1.,0.765913193856979));
#23725=CARTESIAN_POINT('Ctrl Pts',(1.88820926433409,-1.,0.76600483706209));
#23726=CARTESIAN_POINT('Ctrl Pts',(1.88206215302561,-1.,0.766047794851869));
#23727=CARTESIAN_POINT('Ctrl Pts',(1.87592888967886,-1.,0.766042837036759));
#23728=CARTESIAN_POINT('Ctrl Pts',(1.86981398314345,-1.,0.765990708546112));
#23729=CARTESIAN_POINT('Ctrl Pts',(1.86372027063314,-1.,0.765891519092557));
#23730=CARTESIAN_POINT('Ctrl Pts',(1.85764741390391,-1.,0.765744212909305));
#23731=CARTESIAN_POINT('Ctrl Pts',(1.85158945130054,-1.,0.765545710619023));
#23732=CARTESIAN_POINT('Ctrl Pts',(1.8455369887591,-1.,0.765291664861972));
#23733=CARTESIAN_POINT('Ctrl Pts',(1.83948181064823,-1.,0.764978057881688));
#23734=CARTESIAN_POINT('Ctrl Pts',(1.8334207722714,-1.,0.764602549687846));
#23735=CARTESIAN_POINT('Ctrl Pts',(1.8273599120008,-1.,0.764165902606056));
#23736=CARTESIAN_POINT('Ctrl Pts',(1.82131873145297,-1.,0.763673465462854));
#23737=CARTESIAN_POINT('Ctrl Pts',(1.81532118405566,-1.,0.763132003836783));
#23738=CARTESIAN_POINT('Ctrl Pts',(1.80938551463989,-1.,0.762546129464036));
#23739=CARTESIAN_POINT('Ctrl Pts',(1.80351583877334,-1.,0.761915336443516));
#23740=CARTESIAN_POINT('Ctrl Pts',(1.79768986997735,-1.,0.761229695230359));
#23741=CARTESIAN_POINT('Ctrl Pts',(1.79185815610802,-1.,0.760469555880425));
#23742=CARTESIAN_POINT('Ctrl Pts',(1.78596964884526,-1.,0.759614401109868));
#23743=CARTESIAN_POINT('Ctrl Pts',(1.77999411220912,-1.,0.75865062667738));
#23744=CARTESIAN_POINT('Ctrl Pts',(1.77394167108342,-1.,0.757578264077238));
#23745=CARTESIAN_POINT('Ctrl Pts',(1.76789396003141,-1.,0.756421896028403));
#23746=CARTESIAN_POINT('Ctrl Pts',(1.7619781724032,-1.,0.755220979975262));
#23747=CARTESIAN_POINT('Ctrl Pts',(1.75631083600175,-1.,0.75400925402848));
#23748=CARTESIAN_POINT('Ctrl Pts',(1.75095139468809,-1.,0.752797683531377));
#23749=CARTESIAN_POINT('Ctrl Pts',(1.74585086852298,-1.,0.751555614163629));
#23750=CARTESIAN_POINT('Ctrl Pts',(1.74080458266705,-1.,0.750193435979541));
#23751=CARTESIAN_POINT('Ctrl Pts',(1.73550351679848,-1.,0.748582462954855));
#23752=CARTESIAN_POINT('Ctrl Pts',(1.72958533647399,-1.,0.746574710096437));
#23753=CARTESIAN_POINT('Ctrl Pts',(1.7226822991693,-1.,0.744021445433765));
#23754=CARTESIAN_POINT('Ctrl Pts',(1.71447789751927,-1.,0.740795162032088));
#23755=CARTESIAN_POINT('Ctrl Pts',(1.70473309006121,-1.,0.736799665724771));
#23756=CARTESIAN_POINT('Ctrl Pts',(1.69326921975743,-1.,0.731963238697195));
#23757=CARTESIAN_POINT('Ctrl Pts',(1.67996158455503,-1.,0.726235967997433));
#23758=CARTESIAN_POINT('Ctrl Pts',(1.6647288055568,-1.,0.719585433804282));
#23759=CARTESIAN_POINT('Ctrl Pts',(1.64752408832016,-1.,0.711993139355394));
#23760=CARTESIAN_POINT('Ctrl Pts',(1.63216541664676,-1.,0.705159151988319));
#23761=CARTESIAN_POINT('Ctrl Pts',(1.61974673472612,-1.,0.699605146405088));
#23762=CARTESIAN_POINT('Ctrl Pts',(1.61106790958151,-1.,0.695712097881194));
#23763=CARTESIAN_POINT('Ctrl Pts',(1.60662857109684,-1.,0.693717979106306));
#23764=CARTESIAN_POINT('Origin',(0.,-1.,0.));
#23765=CARTESIAN_POINT('Origin',(0.,0.,0.));
#23766=CARTESIAN_POINT('Origin',(0.,2.2,0.));
#23767=CARTESIAN_POINT('Origin',(0.,1.,0.));
#23768=CARTESIAN_POINT('',(-1.4,2.2,1.71450551880629E-16));
#23769=CARTESIAN_POINT('Origin',(0.,2.2,0.));
#23770=CARTESIAN_POINT('',(-1.4,1.,1.71450551880629E-16));
#23771=CARTESIAN_POINT('',(-1.4,1.,1.71450551880629E-16));
#23772=CARTESIAN_POINT('Origin',(0.,1.,0.));
#23773=CARTESIAN_POINT('Origin',(0.,2.2,0.));
#23774=CARTESIAN_POINT('Ctrl Pts',(2.11275013067528,-1.,0.613422273260091));
#23775=CARTESIAN_POINT('Ctrl Pts',(2.11275013067528,1.,0.613422273260091));
#23776=CARTESIAN_POINT('Ctrl Pts',(2.11187554260142,-1.,0.61246736556225));
#23777=CARTESIAN_POINT('Ctrl Pts',(2.11187554260142,1.,0.61246736556225));
#23778=CARTESIAN_POINT('Ctrl Pts',(2.11012443807661,-1.,0.610560911691114));
#23779=CARTESIAN_POINT('Ctrl Pts',(2.11012443807661,1.,0.610560911691114));
#23780=CARTESIAN_POINT('Ctrl Pts',(2.10749199615859,-1.,0.607711315456826));
#23781=CARTESIAN_POINT('Ctrl Pts',(2.10749199615859,1.,0.607711315456826));
#23782=CARTESIAN_POINT('Ctrl Pts',(2.10397049887709,-1.,0.603932030738212));
#23783=CARTESIAN_POINT('Ctrl Pts',(2.10397049887709,1.,0.603932030738212));
#23784=CARTESIAN_POINT('Ctrl Pts',(2.09954930865331,-1.,0.599241616422144));
#23785=CARTESIAN_POINT('Ctrl Pts',(2.09954930865331,1.,0.599241616422144));
#23786=CARTESIAN_POINT('Ctrl Pts',(2.09510876220501,-1.,0.594585006052824));
#23787=CARTESIAN_POINT('Ctrl Pts',(2.09510876220501,1.,0.594585006052824));
#23788=CARTESIAN_POINT('Ctrl Pts',(2.09064881812053,-1.,0.58996236540319));
#23789=CARTESIAN_POINT('Ctrl Pts',(2.09064881812053,1.,0.58996236540319));
#23790=CARTESIAN_POINT('Ctrl Pts',(2.086169437277,-1.,0.585373918990895));
#23791=CARTESIAN_POINT('Ctrl Pts',(2.086169437277,1.,0.585373918990895));
#23792=CARTESIAN_POINT('Ctrl Pts',(2.08167059018138,-1.,0.580819952107257));
#23793=CARTESIAN_POINT('Ctrl Pts',(2.08167059018138,1.,0.580819952107257));
#23794=CARTESIAN_POINT('Ctrl Pts',(2.07715226767361,-1.,0.576300797416275));
#23795=CARTESIAN_POINT('Ctrl Pts',(2.07715226767361,1.,0.576300797416275));
#23796=CARTESIAN_POINT('Ctrl Pts',(2.07261449292757,-1.,0.571816823242411));
#23797=CARTESIAN_POINT('Ctrl Pts',(2.07261449292757,1.,0.571816823242411));
#23798=CARTESIAN_POINT('Ctrl Pts',(2.06805732997383,-1.,0.56736842118123));
#23799=CARTESIAN_POINT('Ctrl Pts',(2.06805732997383,1.,0.56736842118123));
#23800=CARTESIAN_POINT('Ctrl Pts',(2.06348090160697,-1.,0.562955993082574));
#23801=CARTESIAN_POINT('Ctrl Pts',(2.06348090160697,1.,0.562955993082574));
#23802=CARTESIAN_POINT('Ctrl Pts',(2.05888537756571,-1.,0.558579940185468));
#23803=CARTESIAN_POINT('Ctrl Pts',(2.05888537756571,1.,0.558579940185468));
#23804=CARTESIAN_POINT('Ctrl Pts',(2.05427091604482,-1.,0.55424065746411));
#23805=CARTESIAN_POINT('Ctrl Pts',(2.05427091604482,1.,0.55424065746411));
#23806=CARTESIAN_POINT('Ctrl Pts',(2.04963761077974,-1.,0.549938525150342));
#23807=CARTESIAN_POINT('Ctrl Pts',(2.04963761077974,1.,0.549938525150342));
#23808=CARTESIAN_POINT('Ctrl Pts',(2.0449854471456,-1.,0.545673903817349));
#23809=CARTESIAN_POINT('Ctrl Pts',(2.0449854471456,1.,0.545673903817349));
#23810=CARTESIAN_POINT('Ctrl Pts',(2.0403142269048,-1.,0.54144712061552));
#23811=CARTESIAN_POINT('Ctrl Pts',(2.0403142269048,1.,0.54144712061552));
#23812=CARTESIAN_POINT('Ctrl Pts',(2.03562362953993,-1.,0.537258489833135));
#23813=CARTESIAN_POINT('Ctrl Pts',(2.03562362953993,1.,0.537258489833135));
#23814=CARTESIAN_POINT('Ctrl Pts',(2.03091336214401,-1.,0.533108355132905));
#23815=CARTESIAN_POINT('Ctrl Pts',(2.03091336214401,1.,0.533108355132905));
#23816=CARTESIAN_POINT('Ctrl Pts',(2.02618329083289,-1.,0.528997127241911));
#23817=CARTESIAN_POINT('Ctrl Pts',(2.02618329083289,1.,0.528997127241911));
#23818=CARTESIAN_POINT('Ctrl Pts',(2.02143356304712,-1.,0.524925318333519));
#23819=CARTESIAN_POINT('Ctrl Pts',(2.02143356304712,1.,0.524925318333519));
#23820=CARTESIAN_POINT('Ctrl Pts',(2.01666477917305,-1.,0.520893590399429));
#23821=CARTESIAN_POINT('Ctrl Pts',(2.01666477917305,1.,0.520893590399429));
#23822=CARTESIAN_POINT('Ctrl Pts',(2.01187773939257,-1.,0.516902681728733));
#23823=CARTESIAN_POINT('Ctrl Pts',(2.01187773939257,1.,0.516902681728733));
#23824=CARTESIAN_POINT('Ctrl Pts',(2.00707309946955,-1.,0.512953306961814));
#23825=CARTESIAN_POINT('Ctrl Pts',(2.00707309946955,1.,0.512953306961814));
#23826=CARTESIAN_POINT('Ctrl Pts',(2.00225107134733,-1.,0.509046069886152));
#23827=CARTESIAN_POINT('Ctrl Pts',(2.00225107134733,1.,0.509046069886152));
#23828=CARTESIAN_POINT('Ctrl Pts',(1.99741107463567,-1.,0.505181361323011));
#23829=CARTESIAN_POINT('Ctrl Pts',(1.99741107463567,1.,0.505181361323011));
#23830=CARTESIAN_POINT('Ctrl Pts',(1.9925514912615,-1.,0.501359287727129));
#23831=CARTESIAN_POINT('Ctrl Pts',(1.9925514912615,1.,0.501359287727129));
#23832=CARTESIAN_POINT('Ctrl Pts',(1.98767044752929,-1.,0.497579909545564));
#23833=CARTESIAN_POINT('Ctrl Pts',(1.98767044752929,1.,0.497579909545564));
#23834=CARTESIAN_POINT('Ctrl Pts',(1.9827665876182,-1.,0.493843476541493));
#23835=CARTESIAN_POINT('Ctrl Pts',(1.9827665876182,1.,0.493843476541493));
#23836=CARTESIAN_POINT('Ctrl Pts',(1.97783973019229,-1.,0.490150627860955));
#23837=CARTESIAN_POINT('Ctrl Pts',(1.97783973019229,1.,0.490150627860955));
#23838=CARTESIAN_POINT('Ctrl Pts',(1.97289186263272,-1.,0.486502692907661));
#23839=CARTESIAN_POINT('Ctrl Pts',(1.97289186263272,1.,0.486502692907661));
#23840=CARTESIAN_POINT('Ctrl Pts',(1.96792703422358,-1.,0.482901662120687));
#23841=CARTESIAN_POINT('Ctrl Pts',(1.96792703422358,1.,0.482901662120687));
#23842=CARTESIAN_POINT('Ctrl Pts',(1.96294933055938,-1.,0.479349583074846));
#23843=CARTESIAN_POINT('Ctrl Pts',(1.96294933055938,1.,0.479349583074846));
#23844=CARTESIAN_POINT('Ctrl Pts',(1.95796111148175,-1.,0.475848034683172));
#23845=CARTESIAN_POINT('Ctrl Pts',(1.95796111148175,1.,0.475848034683172));
#23846=CARTESIAN_POINT('Ctrl Pts',(1.95296148278136,-1.,0.47239767226408));
#23847=CARTESIAN_POINT('Ctrl Pts',(1.95296148278136,1.,0.47239767226408));
#23848=CARTESIAN_POINT('Ctrl Pts',(1.94794381136524,-1.,0.468997482913158));
#23849=CARTESIAN_POINT('Ctrl Pts',(1.94794381136524,1.,0.468997482913158));
#23850=CARTESIAN_POINT('Ctrl Pts',(1.94289794196205,-1.,0.465645462026065));
#23851=CARTESIAN_POINT('Ctrl Pts',(1.94289794196205,1.,0.465645462026065));
#23852=CARTESIAN_POINT('Ctrl Pts',(1.93781486640834,-1.,0.462340031009087));
#23853=CARTESIAN_POINT('Ctrl Pts',(1.93781486640834,1.,0.462340031009087));
#23854=CARTESIAN_POINT('Ctrl Pts',(1.93269066517936,-1.,0.459081234547932));
#23855=CARTESIAN_POINT('Ctrl Pts',(1.93269066517936,1.,0.459081234547932));
#23856=CARTESIAN_POINT('Ctrl Pts',(1.92753067150461,-1.,0.455872005174336));
#23857=CARTESIAN_POINT('Ctrl Pts',(1.92753067150461,1.,0.455872005174336));
#23858=CARTESIAN_POINT('Ctrl Pts',(1.9223538064847,-1.,0.452719478359356));
#23859=CARTESIAN_POINT('Ctrl Pts',(1.9223538064847,1.,0.452719478359356));
#23860=CARTESIAN_POINT('Ctrl Pts',(1.91718342555717,-1.,0.449632260106572));
#23861=CARTESIAN_POINT('Ctrl Pts',(1.91718342555717,1.,0.449632260106572));
#23862=CARTESIAN_POINT('Ctrl Pts',(1.91203699981095,-1.,0.446617343485651));
#23863=CARTESIAN_POINT('Ctrl Pts',(1.91203699981095,1.,0.446617343485651));
#23864=CARTESIAN_POINT('Ctrl Pts',(1.90691756144906,-1.,0.443677556849171));
#23865=CARTESIAN_POINT('Ctrl Pts',(1.90691756144906,1.,0.443677556849171));
#23866=CARTESIAN_POINT('Ctrl Pts',(1.90180124389137,-1.,0.440807833704161));
#23867=CARTESIAN_POINT('Ctrl Pts',(1.90180124389137,1.,0.440807833704161));
#23868=CARTESIAN_POINT('Ctrl Pts',(1.89663648956549,-1.,0.437995003948443));
#23869=CARTESIAN_POINT('Ctrl Pts',(1.89663648956549,1.,0.437995003948443));
#23870=CARTESIAN_POINT('Ctrl Pts',(1.89136993975585,-1.,0.43522566096358));
#23871=CARTESIAN_POINT('Ctrl Pts',(1.89136993975585,1.,0.43522566096358));
#23872=CARTESIAN_POINT('Ctrl Pts',(1.88596913666828,-1.,0.432493038548833));
#23873=CARTESIAN_POINT('Ctrl Pts',(1.88596913666828,1.,0.432493038548833));
#23874=CARTESIAN_POINT('Ctrl Pts',(1.88044229001778,-1.,0.429803062482217));
#23875=CARTESIAN_POINT('Ctrl Pts',(1.88044229001778,1.,0.429803062482217));
#23876=CARTESIAN_POINT('Ctrl Pts',(1.87486989291333,-1.,0.427183828518743));
#23877=CARTESIAN_POINT('Ctrl Pts',(1.87486989291333,1.,0.427183828518743));
#23878=CARTESIAN_POINT('Ctrl Pts',(1.8693780394412,-1.,0.424678177290876));
#23879=CARTESIAN_POINT('Ctrl Pts',(1.8693780394412,1.,0.424678177290876));
#23880=CARTESIAN_POINT('Ctrl Pts',(1.86408083333863,-1.,0.422327307417885));
#23881=CARTESIAN_POINT('Ctrl Pts',(1.86408083333863,1.,0.422327307417885));
#23882=CARTESIAN_POINT('Ctrl Pts',(1.8590328109667,-1.,0.420157287975583));
#23883=CARTESIAN_POINT('Ctrl Pts',(1.8590328109667,1.,0.420157287975583));
#23884=CARTESIAN_POINT('Ctrl Pts',(1.8541763285645,-1.,0.418164129144046));
#23885=CARTESIAN_POINT('Ctrl Pts',(1.8541763285645,1.,0.418164129144046));
#23886=CARTESIAN_POINT('Ctrl Pts',(1.84929312930314,-1.,0.416300022039885));
#23887=CARTESIAN_POINT('Ctrl Pts',(1.84929312930314,1.,0.416300022039885));
#23888=CARTESIAN_POINT('Ctrl Pts',(1.84405757074218,-1.,0.414487438255542));
#23889=CARTESIAN_POINT('Ctrl Pts',(1.84405757074218,1.,0.414487438255542));
#23890=CARTESIAN_POINT('Ctrl Pts',(1.8380895347617,-1.,0.412633125322945));
#23891=CARTESIAN_POINT('Ctrl Pts',(1.8380895347617,1.,0.412633125322945));
#23892=CARTESIAN_POINT('Ctrl Pts',(1.83100408895047,-1.,0.410641256301276));
#23893=CARTESIAN_POINT('Ctrl Pts',(1.83100408895047,1.,0.410641256301276));
#23894=CARTESIAN_POINT('Ctrl Pts',(1.82247022677562,-1.,0.408428948106228));
#23895=CARTESIAN_POINT('Ctrl Pts',(1.82247022677562,1.,0.408428948106228));
#23896=CARTESIAN_POINT('Ctrl Pts',(1.81223801812013,-1.,0.405933518407176));
#23897=CARTESIAN_POINT('Ctrl Pts',(1.81223801812013,1.,0.405933518407176));
#23898=CARTESIAN_POINT('Ctrl Pts',(1.80012077173238,-1.,0.403107976163396));
#23899=CARTESIAN_POINT('Ctrl Pts',(1.80012077173238,1.,0.403107976163396));
#23900=CARTESIAN_POINT('Ctrl Pts',(1.78598826343754,-1.,0.399919403774156));
#23901=CARTESIAN_POINT('Ctrl Pts',(1.78598826343754,1.,0.399919403774156));
#23902=CARTESIAN_POINT('Ctrl Pts',(1.76975560043442,-1.,0.396346196110688));
#23903=CARTESIAN_POINT('Ctrl Pts',(1.76975560043442,1.,0.396346196110688));
#23904=CARTESIAN_POINT('Ctrl Pts',(1.75137405310193,-1.,0.392375812285396));
#23905=CARTESIAN_POINT('Ctrl Pts',(1.75137405310193,1.,0.392375812285396));
#23906=CARTESIAN_POINT('Ctrl Pts',(1.73493170972829,-1.,0.388877023502615));
#23907=CARTESIAN_POINT('Ctrl Pts',(1.73493170972829,1.,0.388877023502615));
#23908=CARTESIAN_POINT('Ctrl Pts',(1.72162022244582,-1.,0.386070790323281));
#23909=CARTESIAN_POINT('Ctrl Pts',(1.72162022244582,1.,0.386070790323281));
#23910=CARTESIAN_POINT('Ctrl Pts',(1.71231062891398,-1.,0.384119047314215));
#23911=CARTESIAN_POINT('Ctrl Pts',(1.71231062891398,1.,0.384119047314215));
#23912=CARTESIAN_POINT('Ctrl Pts',(1.7075470150345,-1.,0.383122945602004));
#23913=CARTESIAN_POINT('Ctrl Pts',(1.7075470150345,1.,0.383122945602004));
#23914=CARTESIAN_POINT('',(1.7075470150345,1.,0.383122945602004));
#23915=CARTESIAN_POINT('',(1.7075470150345,0.,0.383122945602005));
#23916=CARTESIAN_POINT('',(2.11275013067528,1.,0.613422273260091));
#23917=CARTESIAN_POINT('Ctrl Pts',(2.11275013067528,1.,0.613422273260091));
#23918=CARTESIAN_POINT('Ctrl Pts',(2.11187554260142,1.,0.61246736556225));
#23919=CARTESIAN_POINT('Ctrl Pts',(2.11012443807661,1.,0.610560911691114));
#23920=CARTESIAN_POINT('Ctrl Pts',(2.10749199615859,1.,0.607711315456826));
#23921=CARTESIAN_POINT('Ctrl Pts',(2.10397049887709,1.,0.603932030738212));
#23922=CARTESIAN_POINT('Ctrl Pts',(2.09954930865331,1.,0.599241616422144));
#23923=CARTESIAN_POINT('Ctrl Pts',(2.09510876220501,1.,0.594585006052824));
#23924=CARTESIAN_POINT('Ctrl Pts',(2.09064881812053,1.,0.58996236540319));
#23925=CARTESIAN_POINT('Ctrl Pts',(2.086169437277,1.,0.585373918990895));
#23926=CARTESIAN_POINT('Ctrl Pts',(2.08167059018138,1.,0.580819952107257));
#23927=CARTESIAN_POINT('Ctrl Pts',(2.07715226767361,1.,0.576300797416275));
#23928=CARTESIAN_POINT('Ctrl Pts',(2.07261449292757,1.,0.571816823242411));
#23929=CARTESIAN_POINT('Ctrl Pts',(2.06805732997383,1.,0.56736842118123));
#23930=CARTESIAN_POINT('Ctrl Pts',(2.06348090160697,1.,0.562955993082574));
#23931=CARTESIAN_POINT('Ctrl Pts',(2.05888537756571,1.,0.558579940185468));
#23932=CARTESIAN_POINT('Ctrl Pts',(2.05427091604482,1.,0.55424065746411));
#23933=CARTESIAN_POINT('Ctrl Pts',(2.04963761077974,1.,0.549938525150342));
#23934=CARTESIAN_POINT('Ctrl Pts',(2.0449854471456,1.,0.545673903817349));
#23935=CARTESIAN_POINT('Ctrl Pts',(2.0403142269048,1.,0.54144712061552));
#23936=CARTESIAN_POINT('Ctrl Pts',(2.03562362953993,1.,0.537258489833135));
#23937=CARTESIAN_POINT('Ctrl Pts',(2.03091336214401,1.,0.533108355132905));
#23938=CARTESIAN_POINT('Ctrl Pts',(2.02618329083289,1.,0.528997127241911));
#23939=CARTESIAN_POINT('Ctrl Pts',(2.02143356304712,1.,0.524925318333519));
#23940=CARTESIAN_POINT('Ctrl Pts',(2.01666477917305,1.,0.520893590399429));
#23941=CARTESIAN_POINT('Ctrl Pts',(2.01187773939257,1.,0.516902681728733));
#23942=CARTESIAN_POINT('Ctrl Pts',(2.00707309946955,1.,0.512953306961814));
#23943=CARTESIAN_POINT('Ctrl Pts',(2.00225107134733,1.,0.509046069886152));
#23944=CARTESIAN_POINT('Ctrl Pts',(1.99741107463567,1.,0.505181361323011));
#23945=CARTESIAN_POINT('Ctrl Pts',(1.9925514912615,1.,0.501359287727129));
#23946=CARTESIAN_POINT('Ctrl Pts',(1.98767044752929,1.,0.497579909545564));
#23947=CARTESIAN_POINT('Ctrl Pts',(1.9827665876182,1.,0.493843476541493));
#23948=CARTESIAN_POINT('Ctrl Pts',(1.97783973019229,1.,0.490150627860955));
#23949=CARTESIAN_POINT('Ctrl Pts',(1.97289186263272,1.,0.486502692907661));
#23950=CARTESIAN_POINT('Ctrl Pts',(1.96792703422358,1.,0.482901662120687));
#23951=CARTESIAN_POINT('Ctrl Pts',(1.96294933055938,1.,0.479349583074846));
#23952=CARTESIAN_POINT('Ctrl Pts',(1.95796111148175,1.,0.475848034683172));
#23953=CARTESIAN_POINT('Ctrl Pts',(1.95296148278136,1.,0.47239767226408));
#23954=CARTESIAN_POINT('Ctrl Pts',(1.94794381136524,1.,0.468997482913158));
#23955=CARTESIAN_POINT('Ctrl Pts',(1.94289794196205,1.,0.465645462026065));
#23956=CARTESIAN_POINT('Ctrl Pts',(1.93781486640834,1.,0.462340031009087));
#23957=CARTESIAN_POINT('Ctrl Pts',(1.93269066517936,1.,0.459081234547932));
#23958=CARTESIAN_POINT('Ctrl Pts',(1.92753067150461,1.,0.455872005174336));
#23959=CARTESIAN_POINT('Ctrl Pts',(1.9223538064847,1.,0.452719478359356));
#23960=CARTESIAN_POINT('Ctrl Pts',(1.91718342555717,1.,0.449632260106572));
#23961=CARTESIAN_POINT('Ctrl Pts',(1.91203699981095,1.,0.446617343485651));
#23962=CARTESIAN_POINT('Ctrl Pts',(1.90691756144906,1.,0.443677556849171));
#23963=CARTESIAN_POINT('Ctrl Pts',(1.90180124389137,1.,0.440807833704161));
#23964=CARTESIAN_POINT('Ctrl Pts',(1.89663648956549,1.,0.437995003948443));
#23965=CARTESIAN_POINT('Ctrl Pts',(1.89136993975585,1.,0.43522566096358));
#23966=CARTESIAN_POINT('Ctrl Pts',(1.88596913666828,1.,0.432493038548833));
#23967=CARTESIAN_POINT('Ctrl Pts',(1.88044229001778,1.,0.429803062482217));
#23968=CARTESIAN_POINT('Ctrl Pts',(1.87486989291333,1.,0.427183828518743));
#23969=CARTESIAN_POINT('Ctrl Pts',(1.8693780394412,1.,0.424678177290876));
#23970=CARTESIAN_POINT('Ctrl Pts',(1.86408083333863,1.,0.422327307417885));
#23971=CARTESIAN_POINT('Ctrl Pts',(1.8590328109667,1.,0.420157287975583));
#23972=CARTESIAN_POINT('Ctrl Pts',(1.8541763285645,1.,0.418164129144046));
#23973=CARTESIAN_POINT('Ctrl Pts',(1.84929312930314,1.,0.416300022039885));
#23974=CARTESIAN_POINT('Ctrl Pts',(1.84405757074218,1.,0.414487438255542));
#23975=CARTESIAN_POINT('Ctrl Pts',(1.8380895347617,1.,0.412633125322945));
#23976=CARTESIAN_POINT('Ctrl Pts',(1.83100408895047,1.,0.410641256301276));
#23977=CARTESIAN_POINT('Ctrl Pts',(1.82247022677562,1.,0.408428948106228));
#23978=CARTESIAN_POINT('Ctrl Pts',(1.81223801812013,1.,0.405933518407176));
#23979=CARTESIAN_POINT('Ctrl Pts',(1.80012077173238,1.,0.403107976163396));
#23980=CARTESIAN_POINT('Ctrl Pts',(1.78598826343754,1.,0.399919403774156));
#23981=CARTESIAN_POINT('Ctrl Pts',(1.76975560043442,1.,0.396346196110688));
#23982=CARTESIAN_POINT('Ctrl Pts',(1.75137405310193,1.,0.392375812285396));
#23983=CARTESIAN_POINT('Ctrl Pts',(1.73493170972829,1.,0.388877023502615));
#23984=CARTESIAN_POINT('Ctrl Pts',(1.72162022244582,1.,0.386070790323281));
#23985=CARTESIAN_POINT('Ctrl Pts',(1.71231062891398,1.,0.384119047314215));
#23986=CARTESIAN_POINT('Ctrl Pts',(1.7075470150345,1.,0.383122945602004));
#23987=CARTESIAN_POINT('',(2.11275013067528,0.,0.613422273260091));
#23988=CARTESIAN_POINT('Origin',(2.0698113262342,0.,0.745574324794401));
#23989=CARTESIAN_POINT('',(2.0698113262342,1.,0.745574324794401));
#23990=CARTESIAN_POINT('',(2.11275013067528,1.,0.613422273260091));
#23991=CARTESIAN_POINT('',(2.0698113262342,0.,0.745574324794401));
#23992=CARTESIAN_POINT('Ctrl Pts',(1.60662857109684,-1.,0.693717979106306));
#23993=CARTESIAN_POINT('Ctrl Pts',(1.60662857109684,1.,0.693717979106306));
#23994=CARTESIAN_POINT('Ctrl Pts',(1.61106790958151,-1.,0.695712097881194));
#23995=CARTESIAN_POINT('Ctrl Pts',(1.61106790958151,1.,0.695712097881194));
#23996=CARTESIAN_POINT('Ctrl Pts',(1.61974673472612,-1.,0.699605146405088));
#23997=CARTESIAN_POINT('Ctrl Pts',(1.61974673472612,1.,0.699605146405088));
#23998=CARTESIAN_POINT('Ctrl Pts',(1.63216541664676,-1.,0.705159151988319));
#23999=CARTESIAN_POINT('Ctrl Pts',(1.63216541664676,1.,0.705159151988319));
#24000=CARTESIAN_POINT('Ctrl Pts',(1.64752408832016,-1.,0.711993139355394));
#24001=CARTESIAN_POINT('Ctrl Pts',(1.64752408832016,1.,0.711993139355394));
#24002=CARTESIAN_POINT('Ctrl Pts',(1.6647288055568,-1.,0.719585433804282));
#24003=CARTESIAN_POINT('Ctrl Pts',(1.6647288055568,1.,0.719585433804282));
#24004=CARTESIAN_POINT('Ctrl Pts',(1.67996158455503,-1.,0.726235967997433));
#24005=CARTESIAN_POINT('Ctrl Pts',(1.67996158455503,1.,0.726235967997433));
#24006=CARTESIAN_POINT('Ctrl Pts',(1.69326921975743,-1.,0.731963238697195));
#24007=CARTESIAN_POINT('Ctrl Pts',(1.69326921975743,1.,0.731963238697195));
#24008=CARTESIAN_POINT('Ctrl Pts',(1.70473309006121,-1.,0.736799665724771));
#24009=CARTESIAN_POINT('Ctrl Pts',(1.70473309006121,1.,0.736799665724771));
#24010=CARTESIAN_POINT('Ctrl Pts',(1.71447789751927,-1.,0.740795162032088));
#24011=CARTESIAN_POINT('Ctrl Pts',(1.71447789751927,1.,0.740795162032088));
#24012=CARTESIAN_POINT('Ctrl Pts',(1.7226822991693,-1.,0.744021445433765));
#24013=CARTESIAN_POINT('Ctrl Pts',(1.7226822991693,1.,0.744021445433765));
#24014=CARTESIAN_POINT('Ctrl Pts',(1.72958533647399,-1.,0.746574710096437));
#24015=CARTESIAN_POINT('Ctrl Pts',(1.72958533647399,1.,0.746574710096437));
#24016=CARTESIAN_POINT('Ctrl Pts',(1.73550351679848,-1.,0.748582462954855));
#24017=CARTESIAN_POINT('Ctrl Pts',(1.73550351679848,1.,0.748582462954855));
#24018=CARTESIAN_POINT('Ctrl Pts',(1.74080458266705,-1.,0.750193435979541));
#24019=CARTESIAN_POINT('Ctrl Pts',(1.74080458266705,1.,0.750193435979541));
#24020=CARTESIAN_POINT('Ctrl Pts',(1.74585086852298,-1.,0.751555614163629));
#24021=CARTESIAN_POINT('Ctrl Pts',(1.74585086852298,1.,0.751555614163629));
#24022=CARTESIAN_POINT('Ctrl Pts',(1.75095139468809,-1.,0.752797683531377));
#24023=CARTESIAN_POINT('Ctrl Pts',(1.75095139468809,1.,0.752797683531377));
#24024=CARTESIAN_POINT('Ctrl Pts',(1.75631083600175,-1.,0.75400925402848));
#24025=CARTESIAN_POINT('Ctrl Pts',(1.75631083600175,1.,0.75400925402848));
#24026=CARTESIAN_POINT('Ctrl Pts',(1.7619781724032,-1.,0.755220979975262));
#24027=CARTESIAN_POINT('Ctrl Pts',(1.7619781724032,1.,0.755220979975262));
#24028=CARTESIAN_POINT('Ctrl Pts',(1.76789396003141,-1.,0.756421896028403));
#24029=CARTESIAN_POINT('Ctrl Pts',(1.76789396003141,1.,0.756421896028403));
#24030=CARTESIAN_POINT('Ctrl Pts',(1.77394167108342,-1.,0.757578264077238));
#24031=CARTESIAN_POINT('Ctrl Pts',(1.77394167108342,1.,0.757578264077238));
#24032=CARTESIAN_POINT('Ctrl Pts',(1.77999411220912,-1.,0.75865062667738));
#24033=CARTESIAN_POINT('Ctrl Pts',(1.77999411220912,1.,0.75865062667738));
#24034=CARTESIAN_POINT('Ctrl Pts',(1.78596964884526,-1.,0.759614401109868));
#24035=CARTESIAN_POINT('Ctrl Pts',(1.78596964884526,1.,0.759614401109868));
#24036=CARTESIAN_POINT('Ctrl Pts',(1.79185815610802,-1.,0.760469555880425));
#24037=CARTESIAN_POINT('Ctrl Pts',(1.79185815610802,1.,0.760469555880425));
#24038=CARTESIAN_POINT('Ctrl Pts',(1.79768986997735,-1.,0.761229695230359));
#24039=CARTESIAN_POINT('Ctrl Pts',(1.79768986997735,1.,0.761229695230359));
#24040=CARTESIAN_POINT('Ctrl Pts',(1.80351583877334,-1.,0.761915336443516));
#24041=CARTESIAN_POINT('Ctrl Pts',(1.80351583877334,1.,0.761915336443516));
#24042=CARTESIAN_POINT('Ctrl Pts',(1.80938551463989,-1.,0.762546129464036));
#24043=CARTESIAN_POINT('Ctrl Pts',(1.80938551463989,1.,0.762546129464036));
#24044=CARTESIAN_POINT('Ctrl Pts',(1.81532118405566,-1.,0.763132003836783));
#24045=CARTESIAN_POINT('Ctrl Pts',(1.81532118405566,1.,0.763132003836783));
#24046=CARTESIAN_POINT('Ctrl Pts',(1.82131873145297,-1.,0.763673465462854));
#24047=CARTESIAN_POINT('Ctrl Pts',(1.82131873145297,1.,0.763673465462854));
#24048=CARTESIAN_POINT('Ctrl Pts',(1.8273599120008,-1.,0.764165902606056));
#24049=CARTESIAN_POINT('Ctrl Pts',(1.8273599120008,1.,0.764165902606056));
#24050=CARTESIAN_POINT('Ctrl Pts',(1.8334207722714,-1.,0.764602549687846));
#24051=CARTESIAN_POINT('Ctrl Pts',(1.8334207722714,1.,0.764602549687846));
#24052=CARTESIAN_POINT('Ctrl Pts',(1.83948181064823,-1.,0.764978057881688));
#24053=CARTESIAN_POINT('Ctrl Pts',(1.83948181064823,1.,0.764978057881688));
#24054=CARTESIAN_POINT('Ctrl Pts',(1.8455369887591,-1.,0.765291664861972));
#24055=CARTESIAN_POINT('Ctrl Pts',(1.8455369887591,1.,0.765291664861972));
#24056=CARTESIAN_POINT('Ctrl Pts',(1.85158945130054,-1.,0.765545710619023));
#24057=CARTESIAN_POINT('Ctrl Pts',(1.85158945130054,1.,0.765545710619023));
#24058=CARTESIAN_POINT('Ctrl Pts',(1.85764741390391,-1.,0.765744212909305));
#24059=CARTESIAN_POINT('Ctrl Pts',(1.85764741390391,1.,0.765744212909305));
#24060=CARTESIAN_POINT('Ctrl Pts',(1.86372027063314,-1.,0.765891519092557));
#24061=CARTESIAN_POINT('Ctrl Pts',(1.86372027063314,1.,0.765891519092557));
#24062=CARTESIAN_POINT('Ctrl Pts',(1.86981398314345,-1.,0.765990708546112));
#24063=CARTESIAN_POINT('Ctrl Pts',(1.86981398314345,1.,0.765990708546112));
#24064=CARTESIAN_POINT('Ctrl Pts',(1.87592888967886,-1.,0.766042837036759));
#24065=CARTESIAN_POINT('Ctrl Pts',(1.87592888967886,1.,0.766042837036759));
#24066=CARTESIAN_POINT('Ctrl Pts',(1.88206215302561,-1.,0.766047794851869));
#24067=CARTESIAN_POINT('Ctrl Pts',(1.88206215302561,1.,0.766047794851869));
#24068=CARTESIAN_POINT('Ctrl Pts',(1.88820926433409,-1.,0.76600483706209));
#24069=CARTESIAN_POINT('Ctrl Pts',(1.88820926433409,1.,0.76600483706209));
#24070=CARTESIAN_POINT('Ctrl Pts',(1.89436577771389,-1.,0.765913193856979));
#24071=CARTESIAN_POINT('Ctrl Pts',(1.89436577771389,1.,0.765913193856979));
#24072=CARTESIAN_POINT('Ctrl Pts',(1.90052930393599,-1.,0.765772772593395));
#24073=CARTESIAN_POINT('Ctrl Pts',(1.90052930393599,1.,0.765772772593395));
#24074=CARTESIAN_POINT('Ctrl Pts',(1.90669961402362,-1.,0.765584196937937));
#24075=CARTESIAN_POINT('Ctrl Pts',(1.90669961402362,1.,0.765584196937937));
#24076=CARTESIAN_POINT('Ctrl Pts',(1.91287765805174,-1.,0.765348465884739));
#24077=CARTESIAN_POINT('Ctrl Pts',(1.91287765805174,1.,0.765348465884739));
#24078=CARTESIAN_POINT('Ctrl Pts',(1.91906491634197,-1.,0.765066729667095));
#24079=CARTESIAN_POINT('Ctrl Pts',(1.91906491634197,1.,0.765066729667095));
#24080=CARTESIAN_POINT('Ctrl Pts',(1.92526263537041,-1.,0.764740025488189));
#24081=CARTESIAN_POINT('Ctrl Pts',(1.92526263537041,1.,0.764740025488189));
#24082=CARTESIAN_POINT('Ctrl Pts',(1.93147105496367,-1.,0.76436901067389));
#24083=CARTESIAN_POINT('Ctrl Pts',(1.93147105496367,1.,0.76436901067389));
#24084=CARTESIAN_POINT('Ctrl Pts',(1.93768964875867,-1.,0.763954049121394));
#24085=CARTESIAN_POINT('Ctrl Pts',(1.93768964875867,1.,0.763954049121394));
#24086=CARTESIAN_POINT('Ctrl Pts',(1.94391746617626,-1.,0.763495333538581));
#24087=CARTESIAN_POINT('Ctrl Pts',(1.94391746617626,1.,0.763495333538581));
#24088=CARTESIAN_POINT('Ctrl Pts',(1.95015342590025,-1.,0.762992990878774));
#24089=CARTESIAN_POINT('Ctrl Pts',(1.95015342590025,1.,0.762992990878774));
#24090=CARTESIAN_POINT('Ctrl Pts',(1.95639665309893,-1.,0.762447203806264));
#24091=CARTESIAN_POINT('Ctrl Pts',(1.95639665309893,1.,0.762447203806264));
#24092=CARTESIAN_POINT('Ctrl Pts',(1.96264672744229,-1.,0.761858300014575));
#24093=CARTESIAN_POINT('Ctrl Pts',(1.96264672744229,1.,0.761858300014575));
#24094=CARTESIAN_POINT('Ctrl Pts',(1.96890351582545,-1.,0.761226690483986));
#24095=CARTESIAN_POINT('Ctrl Pts',(1.96890351582545,1.,0.761226690483986));
#24096=CARTESIAN_POINT('Ctrl Pts',(1.97516705321521,-1.,0.760552825409856));
#24097=CARTESIAN_POINT('Ctrl Pts',(1.97516705321521,1.,0.760552825409856));
#24098=CARTESIAN_POINT('Ctrl Pts',(1.98143741418156,-1.,0.759837147452135));
#24099=CARTESIAN_POINT('Ctrl Pts',(1.98143741418156,1.,0.759837147452135));
#24100=CARTESIAN_POINT('Ctrl Pts',(1.98771456680806,-1.,0.759080037802243));
#24101=CARTESIAN_POINT('Ctrl Pts',(1.98771456680806,1.,0.759080037802243));
#24102=CARTESIAN_POINT('Ctrl Pts',(1.9939983109871,-1.,0.758281796766377));
#24103=CARTESIAN_POINT('Ctrl Pts',(1.9939983109871,1.,0.758281796766377));
#24104=CARTESIAN_POINT('Ctrl Pts',(2.00028834739072,-1.,0.757442676862342));
#24105=CARTESIAN_POINT('Ctrl Pts',(2.00028834739072,1.,0.757442676862342));
#24106=CARTESIAN_POINT('Ctrl Pts',(2.00658431587682,-1.,0.756562904646496));
#24107=CARTESIAN_POINT('Ctrl Pts',(2.00658431587682,1.,0.756562904646496));
#24108=CARTESIAN_POINT('Ctrl Pts',(2.01288584328149,-1.,0.755642704958101));
#24109=CARTESIAN_POINT('Ctrl Pts',(2.01288584328149,1.,0.755642704958101));
#24110=CARTESIAN_POINT('Ctrl Pts',(2.01919259406003,-1.,0.75468233072352));
#24111=CARTESIAN_POINT('Ctrl Pts',(2.01919259406003,1.,0.75468233072352));
#24112=CARTESIAN_POINT('Ctrl Pts',(2.02550428623587,-1.,0.753682061113766));
#24113=CARTESIAN_POINT('Ctrl Pts',(2.02550428623587,1.,0.753682061113766));
#24114=CARTESIAN_POINT('Ctrl Pts',(2.03182068456467,-1.,0.752642180488104));
#24115=CARTESIAN_POINT('Ctrl Pts',(2.03182068456467,1.,0.752642180488104));
#24116=CARTESIAN_POINT('Ctrl Pts',(2.03814160092173,-1.,0.751562963361384));
#24117=CARTESIAN_POINT('Ctrl Pts',(2.03814160092173,1.,0.751562963361384));
#24118=CARTESIAN_POINT('Ctrl Pts',(2.04446689147754,-1.,0.750444657874758));
#24119=CARTESIAN_POINT('Ctrl Pts',(2.04446689147754,1.,0.750444657874758));
#24120=CARTESIAN_POINT('Ctrl Pts',(2.05079645591606,-1.,0.749287468663053));
#24121=CARTESIAN_POINT('Ctrl Pts',(2.05079645591606,1.,0.749287468663053));
#24122=CARTESIAN_POINT('Ctrl Pts',(2.05713023030263,-1.,0.748091554181101));
#24123=CARTESIAN_POINT('Ctrl Pts',(2.05713023030263,1.,0.748091554181101));
#24124=CARTESIAN_POINT('Ctrl Pts',(2.06220058927162,-1.,0.747103932785504));
#24125=CARTESIAN_POINT('Ctrl Pts',(2.06220058927162,1.,0.747103932785504));
#24126=CARTESIAN_POINT('Ctrl Pts',(2.06600523016401,-1.,0.746345871542696));
#24127=CARTESIAN_POINT('Ctrl Pts',(2.06600523016401,1.,0.746345871542696));
#24128=CARTESIAN_POINT('Ctrl Pts',(2.06854248895575,-1.,0.74583279137781));
#24129=CARTESIAN_POINT('Ctrl Pts',(2.06854248895575,1.,0.74583279137781));
#24130=CARTESIAN_POINT('Ctrl Pts',(2.0698113262342,-1.,0.745574324794401));
#24131=CARTESIAN_POINT('Ctrl Pts',(2.0698113262342,1.,0.745574324794401));
#24132=CARTESIAN_POINT('',(1.60662857109684,1.,0.693717979106306));
#24133=CARTESIAN_POINT('Ctrl Pts',(1.60662857109684,1.,0.693717979106306));
#24134=CARTESIAN_POINT('Ctrl Pts',(1.61106790958151,1.,0.695712097881194));
#24135=CARTESIAN_POINT('Ctrl Pts',(1.61974673472612,1.,0.699605146405088));
#24136=CARTESIAN_POINT('Ctrl Pts',(1.63216541664676,1.,0.705159151988319));
#24137=CARTESIAN_POINT('Ctrl Pts',(1.64752408832016,1.,0.711993139355394));
#24138=CARTESIAN_POINT('Ctrl Pts',(1.6647288055568,1.,0.719585433804282));
#24139=CARTESIAN_POINT('Ctrl Pts',(1.67996158455503,1.,0.726235967997433));
#24140=CARTESIAN_POINT('Ctrl Pts',(1.69326921975743,1.,0.731963238697195));
#24141=CARTESIAN_POINT('Ctrl Pts',(1.70473309006121,1.,0.736799665724771));
#24142=CARTESIAN_POINT('Ctrl Pts',(1.71447789751927,1.,0.740795162032088));
#24143=CARTESIAN_POINT('Ctrl Pts',(1.7226822991693,1.,0.744021445433765));
#24144=CARTESIAN_POINT('Ctrl Pts',(1.72958533647399,1.,0.746574710096437));
#24145=CARTESIAN_POINT('Ctrl Pts',(1.73550351679848,1.,0.748582462954855));
#24146=CARTESIAN_POINT('Ctrl Pts',(1.74080458266705,1.,0.750193435979541));
#24147=CARTESIAN_POINT('Ctrl Pts',(1.74585086852298,1.,0.751555614163629));
#24148=CARTESIAN_POINT('Ctrl Pts',(1.75095139468809,1.,0.752797683531377));
#24149=CARTESIAN_POINT('Ctrl Pts',(1.75631083600175,1.,0.75400925402848));
#24150=CARTESIAN_POINT('Ctrl Pts',(1.7619781724032,1.,0.755220979975262));
#24151=CARTESIAN_POINT('Ctrl Pts',(1.76789396003141,1.,0.756421896028403));
#24152=CARTESIAN_POINT('Ctrl Pts',(1.77394167108342,1.,0.757578264077238));
#24153=CARTESIAN_POINT('Ctrl Pts',(1.77999411220912,1.,0.75865062667738));
#24154=CARTESIAN_POINT('Ctrl Pts',(1.78596964884526,1.,0.759614401109868));
#24155=CARTESIAN_POINT('Ctrl Pts',(1.79185815610802,1.,0.760469555880425));
#24156=CARTESIAN_POINT('Ctrl Pts',(1.79768986997735,1.,0.761229695230359));
#24157=CARTESIAN_POINT('Ctrl Pts',(1.80351583877334,1.,0.761915336443516));
#24158=CARTESIAN_POINT('Ctrl Pts',(1.80938551463989,1.,0.762546129464036));
#24159=CARTESIAN_POINT('Ctrl Pts',(1.81532118405566,1.,0.763132003836783));
#24160=CARTESIAN_POINT('Ctrl Pts',(1.82131873145297,1.,0.763673465462854));
#24161=CARTESIAN_POINT('Ctrl Pts',(1.8273599120008,1.,0.764165902606056));
#24162=CARTESIAN_POINT('Ctrl Pts',(1.8334207722714,1.,0.764602549687846));
#24163=CARTESIAN_POINT('Ctrl Pts',(1.83948181064823,1.,0.764978057881688));
#24164=CARTESIAN_POINT('Ctrl Pts',(1.8455369887591,1.,0.765291664861972));
#24165=CARTESIAN_POINT('Ctrl Pts',(1.85158945130054,1.,0.765545710619023));
#24166=CARTESIAN_POINT('Ctrl Pts',(1.85764741390391,1.,0.765744212909305));
#24167=CARTESIAN_POINT('Ctrl Pts',(1.86372027063314,1.,0.765891519092557));
#24168=CARTESIAN_POINT('Ctrl Pts',(1.86981398314345,1.,0.765990708546112));
#24169=CARTESIAN_POINT('Ctrl Pts',(1.87592888967886,1.,0.766042837036759));
#24170=CARTESIAN_POINT('Ctrl Pts',(1.88206215302561,1.,0.766047794851869));
#24171=CARTESIAN_POINT('Ctrl Pts',(1.88820926433409,1.,0.76600483706209));
#24172=CARTESIAN_POINT('Ctrl Pts',(1.89436577771389,1.,0.765913193856979));
#24173=CARTESIAN_POINT('Ctrl Pts',(1.90052930393599,1.,0.765772772593395));
#24174=CARTESIAN_POINT('Ctrl Pts',(1.90669961402362,1.,0.765584196937937));
#24175=CARTESIAN_POINT('Ctrl Pts',(1.91287765805174,1.,0.765348465884739));
#24176=CARTESIAN_POINT('Ctrl Pts',(1.91906491634197,1.,0.765066729667095));
#24177=CARTESIAN_POINT('Ctrl Pts',(1.92526263537041,1.,0.764740025488189));
#24178=CARTESIAN_POINT('Ctrl Pts',(1.93147105496367,1.,0.76436901067389));
#24179=CARTESIAN_POINT('Ctrl Pts',(1.93768964875867,1.,0.763954049121394));
#24180=CARTESIAN_POINT('Ctrl Pts',(1.94391746617626,1.,0.763495333538581));
#24181=CARTESIAN_POINT('Ctrl Pts',(1.95015342590025,1.,0.762992990878774));
#24182=CARTESIAN_POINT('Ctrl Pts',(1.95639665309893,1.,0.762447203806264));
#24183=CARTESIAN_POINT('Ctrl Pts',(1.96264672744229,1.,0.761858300014575));
#24184=CARTESIAN_POINT('Ctrl Pts',(1.96890351582545,1.,0.761226690483986));
#24185=CARTESIAN_POINT('Ctrl Pts',(1.97516705321521,1.,0.760552825409856));
#24186=CARTESIAN_POINT('Ctrl Pts',(1.98143741418156,1.,0.759837147452135));
#24187=CARTESIAN_POINT('Ctrl Pts',(1.98771456680806,1.,0.759080037802243));
#24188=CARTESIAN_POINT('Ctrl Pts',(1.9939983109871,1.,0.758281796766377));
#24189=CARTESIAN_POINT('Ctrl Pts',(2.00028834739072,1.,0.757442676862342));
#24190=CARTESIAN_POINT('Ctrl Pts',(2.00658431587682,1.,0.756562904646496));
#24191=CARTESIAN_POINT('Ctrl Pts',(2.01288584328149,1.,0.755642704958101));
#24192=CARTESIAN_POINT('Ctrl Pts',(2.01919259406003,1.,0.75468233072352));
#24193=CARTESIAN_POINT('Ctrl Pts',(2.02550428623587,1.,0.753682061113766));
#24194=CARTESIAN_POINT('Ctrl Pts',(2.03182068456467,1.,0.752642180488104));
#24195=CARTESIAN_POINT('Ctrl Pts',(2.03814160092173,1.,0.751562963361384));
#24196=CARTESIAN_POINT('Ctrl Pts',(2.04446689147754,1.,0.750444657874758));
#24197=CARTESIAN_POINT('Ctrl Pts',(2.05079645591606,1.,0.749287468663053));
#24198=CARTESIAN_POINT('Ctrl Pts',(2.05713023030263,1.,0.748091554181101));
#24199=CARTESIAN_POINT('Ctrl Pts',(2.06220058927162,1.,0.747103932785504));
#24200=CARTESIAN_POINT('Ctrl Pts',(2.06600523016401,1.,0.746345871542696));
#24201=CARTESIAN_POINT('Ctrl Pts',(2.06854248895575,1.,0.74583279137781));
#24202=CARTESIAN_POINT('Ctrl Pts',(2.0698113262342,1.,0.745574324794401));
#24203=CARTESIAN_POINT('',(1.60662857109684,0.,0.693717979106305));
#24204=CARTESIAN_POINT('Origin',(0.,0.,0.));
#24205=CARTESIAN_POINT('',(1.5055822144029,1.,0.892032620296856));
#24206=CARTESIAN_POINT('Origin',(0.,1.,0.));
#24207=CARTESIAN_POINT('',(1.5055822144029,0.,0.892032620296855));
#24208=CARTESIAN_POINT('Ctrl Pts',(1.81978687191668,-1.,1.23627494547115));
#24209=CARTESIAN_POINT('Ctrl Pts',(1.81978687191668,1.,1.23627494547115));
#24210=CARTESIAN_POINT('Ctrl Pts',(1.81925017193666,-1.,1.23509651170476));
#24211=CARTESIAN_POINT('Ctrl Pts',(1.81925017193666,1.,1.23509651170476));
#24212=CARTESIAN_POINT('Ctrl Pts',(1.81817389921279,-1.,1.2327422452705));
#24213=CARTESIAN_POINT('Ctrl Pts',(1.81817389921279,1.,1.2327422452705));
#24214=CARTESIAN_POINT('Ctrl Pts',(1.8165508718364,-1.,1.2292186489137));
#24215=CARTESIAN_POINT('Ctrl Pts',(1.8165508718364,1.,1.2292186489137));
#24216=CARTESIAN_POINT('Ctrl Pts',(1.81436959210434,-1.,1.2245361330495));
#24217=CARTESIAN_POINT('Ctrl Pts',(1.81436959210434,1.,1.2245361330495));
#24218=CARTESIAN_POINT('Ctrl Pts',(1.81161420806656,-1.,1.21870906103557));
#24219=CARTESIAN_POINT('Ctrl Pts',(1.81161420806656,1.,1.21870906103557));
#24220=CARTESIAN_POINT('Ctrl Pts',(1.80882996917129,-1.,1.21290815708314));
#24221=CARTESIAN_POINT('Ctrl Pts',(1.80882996917129,1.,1.21290815708314));
#24222=CARTESIAN_POINT('Ctrl Pts',(1.80601678480707,-1.,1.20713356605475));
#24223=CARTESIAN_POINT('Ctrl Pts',(1.80601678480707,1.,1.20713356605475));
#24224=CARTESIAN_POINT('Ctrl Pts',(1.80317454838603,-1.,1.20138548938974));
#24225=CARTESIAN_POINT('Ctrl Pts',(1.80317454838603,1.,1.20138548938974));
#24226=CARTESIAN_POINT('Ctrl Pts',(1.80030314369879,-1.,1.19566418930242));
#24227=CARTESIAN_POINT('Ctrl Pts',(1.80030314369879,1.,1.19566418930242));
#24228=CARTESIAN_POINT('Ctrl Pts',(1.79740245923478,-1.,1.18996997934445));
#24229=CARTESIAN_POINT('Ctrl Pts',(1.79740245923478,1.,1.18996997934445));
#24230=CARTESIAN_POINT('Ctrl Pts',(1.79447240321515,-1.,1.18430321697432));
#24231=CARTESIAN_POINT('Ctrl Pts',(1.79447240321515,1.,1.18430321697432));
#24232=CARTESIAN_POINT('Ctrl Pts',(1.79151291552689,-1.,1.17866429440809));
#24233=CARTESIAN_POINT('Ctrl Pts',(1.79151291552689,1.,1.17866429440809));
#24234=CARTESIAN_POINT('Ctrl Pts',(1.78852398877616,-1.,1.17305363177328));
#24235=CARTESIAN_POINT('Ctrl Pts',(1.78852398877616,1.,1.17305363177328));
#24236=CARTESIAN_POINT('Ctrl Pts',(1.78550566040443,-1.,1.16747166312303));
#24237=CARTESIAN_POINT('Ctrl Pts',(1.78550566040443,1.,1.16747166312303));
#24238=CARTESIAN_POINT('Ctrl Pts',(1.78245795881009,-1.,1.16191881298499));
#24239=CARTESIAN_POINT('Ctrl Pts',(1.78245795881009,1.,1.16191881298499));
#24240=CARTESIAN_POINT('Ctrl Pts',(1.77938085564275,-1.,1.15639547194698));
#24241=CARTESIAN_POINT('Ctrl Pts',(1.77938085564275,1.,1.15639547194698));
#24242=CARTESIAN_POINT('Ctrl Pts',(1.7762742255701,-1.,1.15090197841515));
#24243=CARTESIAN_POINT('Ctrl Pts',(1.7762742255701,1.,1.15090197841515));
#24244=CARTESIAN_POINT('Ctrl Pts',(1.77313777896194,-1.,1.1454385822692));
#24245=CARTESIAN_POINT('Ctrl Pts',(1.77313777896194,1.,1.1454385822692));
#24246=CARTESIAN_POINT('Ctrl Pts',(1.76997111386769,-1.,1.14000548336975));
#24247=CARTESIAN_POINT('Ctrl Pts',(1.76997111386769,1.,1.14000548336975));
#24248=CARTESIAN_POINT('Ctrl Pts',(1.76677384551862,-1.,1.1346029180462));
#24249=CARTESIAN_POINT('Ctrl Pts',(1.76677384551862,1.,1.1346029180462));
#24250=CARTESIAN_POINT('Ctrl Pts',(1.7635457196617,-1.,1.12923123555075));
#24251=CARTESIAN_POINT('Ctrl Pts',(1.7635457196617,1.,1.12923123555075));
#24252=CARTESIAN_POINT('Ctrl Pts',(1.76028671825096,-1.,1.12389096855086));
#24253=CARTESIAN_POINT('Ctrl Pts',(1.76028671825096,1.,1.12389096855086));
#24254=CARTESIAN_POINT('Ctrl Pts',(1.75699720772105,-1.,1.11858293216763));
#24255=CARTESIAN_POINT('Ctrl Pts',(1.75699720772105,1.,1.11858293216763));
#24256=CARTESIAN_POINT('Ctrl Pts',(1.7536777209463,-1.,1.11330807582551));
#24257=CARTESIAN_POINT('Ctrl Pts',(1.7536777209463,1.,1.11330807582551));
#24258=CARTESIAN_POINT('Ctrl Pts',(1.7503286607592,-1.,1.10806728183007));
#24259=CARTESIAN_POINT('Ctrl Pts',(1.7503286607592,1.,1.10806728183007));
#24260=CARTESIAN_POINT('Ctrl Pts',(1.74695004214923,-1.,1.10286118991143));
#24261=CARTESIAN_POINT('Ctrl Pts',(1.74695004214923,1.,1.10286118991143));
#24262=CARTESIAN_POINT('Ctrl Pts',(1.74354119236208,-1.,1.09768999241226));
#24263=CARTESIAN_POINT('Ctrl Pts',(1.74354119236208,1.,1.09768999241226));
#24264=CARTESIAN_POINT('Ctrl Pts',(1.74010053962247,-1.,1.09255329056493));
#24265=CARTESIAN_POINT('Ctrl Pts',(1.74010053962247,1.,1.09255329056493));
#24266=CARTESIAN_POINT('Ctrl Pts',(1.73662628326091,-1.,1.08745056285427));
#24267=CARTESIAN_POINT('Ctrl Pts',(1.73662628326091,1.,1.08745056285427));
#24268=CARTESIAN_POINT('Ctrl Pts',(1.73311705663407,-1.,1.08238162784749));
#24269=CARTESIAN_POINT('Ctrl Pts',(1.73311705663407,1.,1.08238162784749));
#24270=CARTESIAN_POINT('Ctrl Pts',(1.72957248977424,-1.,1.0773470373727));
#24271=CARTESIAN_POINT('Ctrl Pts',(1.72957248977424,1.,1.0773470373727));
#24272=CARTESIAN_POINT('Ctrl Pts',(1.72599406198488,-1.,1.07234866990252));
#24273=CARTESIAN_POINT('Ctrl Pts',(1.72599406198488,1.,1.07234866990252));
#24274=CARTESIAN_POINT('Ctrl Pts',(1.72238500928453,-1.,1.06738966975462));
#24275=CARTESIAN_POINT('Ctrl Pts',(1.72238500928453,1.,1.06738966975462));
#24276=CARTESIAN_POINT('Ctrl Pts',(1.71874858456904,-1.,1.06247324680647));
#24277=CARTESIAN_POINT('Ctrl Pts',(1.71874858456904,1.,1.06247324680647));
#24278=CARTESIAN_POINT('Ctrl Pts',(1.7150865442702,-1.,1.05760163192479));
#24279=CARTESIAN_POINT('Ctrl Pts',(1.7150865442702,1.,1.05760163192479));
#24280=CARTESIAN_POINT('Ctrl Pts',(1.71139783543989,-1.,1.05277517202855));
#24281=CARTESIAN_POINT('Ctrl Pts',(1.71139783543989,1.,1.05277517202855));
#24282=CARTESIAN_POINT('Ctrl Pts',(1.70767646263649,-1.,1.04799085404995));
#24283=CARTESIAN_POINT('Ctrl Pts',(1.70767646263649,1.,1.04799085404995));
#24284=CARTESIAN_POINT('Ctrl Pts',(1.70391338707982,-1.,1.04324363334554));
#24285=CARTESIAN_POINT('Ctrl Pts',(1.70391338707982,1.,1.04324363334554));
#24286=CARTESIAN_POINT('Ctrl Pts',(1.70010052930962,-1.,1.03852922490789));
#24287=CARTESIAN_POINT('Ctrl Pts',(1.70010052930962,1.,1.03852922490789));
#24288=CARTESIAN_POINT('Ctrl Pts',(1.69623414782771,-1.,1.03384646003588));
#24289=CARTESIAN_POINT('Ctrl Pts',(1.69623414782771,1.,1.03384646003588));
#24290=CARTESIAN_POINT('Ctrl Pts',(1.69231840863458,-1.,1.02919977579147));
#24291=CARTESIAN_POINT('Ctrl Pts',(1.69231840863458,1.,1.02919977579147));
#24292=CARTESIAN_POINT('Ctrl Pts',(1.68836910178447,-1.,1.02460180535255));
#24293=CARTESIAN_POINT('Ctrl Pts',(1.68836910178447,1.,1.02460180535255));
#24294=CARTESIAN_POINT('Ctrl Pts',(1.68440578021706,-1.,1.02006795074201));
#24295=CARTESIAN_POINT('Ctrl Pts',(1.68440578021706,1.,1.02006795074201));
#24296=CARTESIAN_POINT('Ctrl Pts',(1.68044289894798,-1.,1.01561026162773));
#24297=CARTESIAN_POINT('Ctrl Pts',(1.68044289894798,1.,1.01561026162773));
#24298=CARTESIAN_POINT('Ctrl Pts',(1.67648246776464,-1.,1.01123236493511));
#24299=CARTESIAN_POINT('Ctrl Pts',(1.67648246776464,1.,1.01123236493511));
#24300=CARTESIAN_POINT('Ctrl Pts',(1.67250335383293,-1.,1.00692206696414));
#24301=CARTESIAN_POINT('Ctrl Pts',(1.67250335383293,1.,1.00692206696414));
#24302=CARTESIAN_POINT('Ctrl Pts',(1.66846059277303,-1.,1.00265091003727));
#24303=CARTESIAN_POINT('Ctrl Pts',(1.66846059277303,1.,1.00265091003727));
#24304=CARTESIAN_POINT('Ctrl Pts',(1.66430758030376,-1.,0.998389654952758));
#24305=CARTESIAN_POINT('Ctrl Pts',(1.66430758030376,1.,0.998389654952758));
#24306=CARTESIAN_POINT('Ctrl Pts',(1.66001553809947,-1.,0.994121836661306));
#24307=CARTESIAN_POINT('Ctrl Pts',(1.66001553809947,1.,0.994121836661306));
#24308=CARTESIAN_POINT('Ctrl Pts',(1.65559044289699,-1.,0.989855627854165));
#24309=CARTESIAN_POINT('Ctrl Pts',(1.65559044289699,1.,0.989855627854165));
#24310=CARTESIAN_POINT('Ctrl Pts',(1.65110016612638,-1.,0.985642622920821));
#24311=CARTESIAN_POINT('Ctrl Pts',(1.65110016612638,1.,0.985642622920821));
#24312=CARTESIAN_POINT('Ctrl Pts',(1.64665139190656,-1.,0.981562530939489));
#24313=CARTESIAN_POINT('Ctrl Pts',(1.64665139190656,1.,0.981562530939489));
#24314=CARTESIAN_POINT('Ctrl Pts',(1.64233990826687,-1.,0.977689794119417));
#24315=CARTESIAN_POINT('Ctrl Pts',(1.64233990826687,1.,0.977689794119417));
#24316=CARTESIAN_POINT('Ctrl Pts',(1.63820952658144,-1.,0.974066058287419));
#24317=CARTESIAN_POINT('Ctrl Pts',(1.63820952658144,1.,0.974066058287419));
#24318=CARTESIAN_POINT('Ctrl Pts',(1.63420665729798,-1.,0.970669715997509));
#24319=CARTESIAN_POINT('Ctrl Pts',(1.63420665729798,1.,0.970669715997509));
#24320=CARTESIAN_POINT('Ctrl Pts',(1.63013849959461,-1.,0.967387853230345));
#24321=CARTESIAN_POINT('Ctrl Pts',(1.63013849959461,1.,0.967387853230345));
#24322=CARTESIAN_POINT('Ctrl Pts',(1.62571930670187,-1.,0.964046107040536));
#24323=CARTESIAN_POINT('Ctrl Pts',(1.62571930670187,1.,0.964046107040536));
#24324=CARTESIAN_POINT('Ctrl Pts',(1.62061638140221,-1.,0.960438326101729));
#24325=CARTESIAN_POINT('Ctrl Pts',(1.62061638140221,1.,0.960438326101729));
#24326=CARTESIAN_POINT('Ctrl Pts',(1.61449324337085,-1.,0.956354422920671));
#24327=CARTESIAN_POINT('Ctrl Pts',(1.61449324337085,1.,0.956354422920671));
#24328=CARTESIAN_POINT('Ctrl Pts',(1.60706069896936,-1.,0.951613284356035));
#24329=CARTESIAN_POINT('Ctrl Pts',(1.60706069896936,1.,0.951613284356035));
#24330=CARTESIAN_POINT('Ctrl Pts',(1.59810042043673,-1.,0.946078063315257));
#24331=CARTESIAN_POINT('Ctrl Pts',(1.59810042043673,1.,0.946078063315257));
#24332=CARTESIAN_POINT('Ctrl Pts',(1.58744937487176,-1.,0.939646377893399));
#24333=CARTESIAN_POINT('Ctrl Pts',(1.58744937487176,1.,0.939646377893399));
#24334=CARTESIAN_POINT('Ctrl Pts',(1.57499388382243,-1.,0.932246680108685));
#24335=CARTESIAN_POINT('Ctrl Pts',(1.57499388382243,1.,0.932246680108685));
#24336=CARTESIAN_POINT('Ctrl Pts',(1.56065988578893,-1.,0.923832188944341));
#24337=CARTESIAN_POINT('Ctrl Pts',(1.56065988578893,1.,0.923832188944341));
#24338=CARTESIAN_POINT('Ctrl Pts',(1.54440491149498,-1.,0.914375919026456));
#24339=CARTESIAN_POINT('Ctrl Pts',(1.54440491149498,1.,0.914375919026456));
#24340=CARTESIAN_POINT('Ctrl Pts',(1.52984849887993,-1.,0.905967409625651));
#24341=CARTESIAN_POINT('Ctrl Pts',(1.52984849887993,1.,0.905967409625651));
#24342=CARTESIAN_POINT('Ctrl Pts',(1.51805569590094,-1.,0.899185047483511));
#24343=CARTESIAN_POINT('Ctrl Pts',(1.51805569590094,1.,0.899185047483511));
#24344=CARTESIAN_POINT('Ctrl Pts',(1.50980486806688,-1.,0.894452006964544));
#24345=CARTESIAN_POINT('Ctrl Pts',(1.50980486806688,1.,0.894452006964544));
#24346=CARTESIAN_POINT('Ctrl Pts',(1.5055822144029,-1.,0.892032620296856));
#24347=CARTESIAN_POINT('Ctrl Pts',(1.5055822144029,1.,0.892032620296856));
#24348=CARTESIAN_POINT('',(1.81978687191668,1.,1.23627494547115));
#24349=CARTESIAN_POINT('Ctrl Pts',(1.81978687191668,1.,1.23627494547115));
#24350=CARTESIAN_POINT('Ctrl Pts',(1.81925017193666,1.,1.23509651170476));
#24351=CARTESIAN_POINT('Ctrl Pts',(1.81817389921279,1.,1.2327422452705));
#24352=CARTESIAN_POINT('Ctrl Pts',(1.8165508718364,1.,1.2292186489137));
#24353=CARTESIAN_POINT('Ctrl Pts',(1.81436959210434,1.,1.2245361330495));
#24354=CARTESIAN_POINT('Ctrl Pts',(1.81161420806656,1.,1.21870906103557));
#24355=CARTESIAN_POINT('Ctrl Pts',(1.80882996917129,1.,1.21290815708314));
#24356=CARTESIAN_POINT('Ctrl Pts',(1.80601678480707,1.,1.20713356605475));
#24357=CARTESIAN_POINT('Ctrl Pts',(1.80317454838603,1.,1.20138548938974));
#24358=CARTESIAN_POINT('Ctrl Pts',(1.80030314369879,1.,1.19566418930242));
#24359=CARTESIAN_POINT('Ctrl Pts',(1.79740245923478,1.,1.18996997934445));
#24360=CARTESIAN_POINT('Ctrl Pts',(1.79447240321515,1.,1.18430321697432));
#24361=CARTESIAN_POINT('Ctrl Pts',(1.79151291552689,1.,1.17866429440809));
#24362=CARTESIAN_POINT('Ctrl Pts',(1.78852398877616,1.,1.17305363177328));
#24363=CARTESIAN_POINT('Ctrl Pts',(1.78550566040443,1.,1.16747166312303));
#24364=CARTESIAN_POINT('Ctrl Pts',(1.78245795881009,1.,1.16191881298499));
#24365=CARTESIAN_POINT('Ctrl Pts',(1.77938085564275,1.,1.15639547194698));
#24366=CARTESIAN_POINT('Ctrl Pts',(1.7762742255701,1.,1.15090197841515));
#24367=CARTESIAN_POINT('Ctrl Pts',(1.77313777896194,1.,1.1454385822692));
#24368=CARTESIAN_POINT('Ctrl Pts',(1.76997111386769,1.,1.14000548336975));
#24369=CARTESIAN_POINT('Ctrl Pts',(1.76677384551862,1.,1.1346029180462));
#24370=CARTESIAN_POINT('Ctrl Pts',(1.7635457196617,1.,1.12923123555075));
#24371=CARTESIAN_POINT('Ctrl Pts',(1.76028671825096,1.,1.12389096855086));
#24372=CARTESIAN_POINT('Ctrl Pts',(1.75699720772105,1.,1.11858293216763));
#24373=CARTESIAN_POINT('Ctrl Pts',(1.7536777209463,1.,1.11330807582551));
#24374=CARTESIAN_POINT('Ctrl Pts',(1.7503286607592,1.,1.10806728183007));
#24375=CARTESIAN_POINT('Ctrl Pts',(1.74695004214923,1.,1.10286118991143));
#24376=CARTESIAN_POINT('Ctrl Pts',(1.74354119236208,1.,1.09768999241226));
#24377=CARTESIAN_POINT('Ctrl Pts',(1.74010053962247,1.,1.09255329056493));
#24378=CARTESIAN_POINT('Ctrl Pts',(1.73662628326091,1.,1.08745056285427));
#24379=CARTESIAN_POINT('Ctrl Pts',(1.73311705663407,1.,1.08238162784749));
#24380=CARTESIAN_POINT('Ctrl Pts',(1.72957248977424,1.,1.0773470373727));
#24381=CARTESIAN_POINT('Ctrl Pts',(1.72599406198488,1.,1.07234866990252));
#24382=CARTESIAN_POINT('Ctrl Pts',(1.72238500928453,1.,1.06738966975462));
#24383=CARTESIAN_POINT('Ctrl Pts',(1.71874858456904,1.,1.06247324680647));
#24384=CARTESIAN_POINT('Ctrl Pts',(1.7150865442702,1.,1.05760163192479));
#24385=CARTESIAN_POINT('Ctrl Pts',(1.71139783543989,1.,1.05277517202855));
#24386=CARTESIAN_POINT('Ctrl Pts',(1.70767646263649,1.,1.04799085404995));
#24387=CARTESIAN_POINT('Ctrl Pts',(1.70391338707982,1.,1.04324363334554));
#24388=CARTESIAN_POINT('Ctrl Pts',(1.70010052930962,1.,1.03852922490789));
#24389=CARTESIAN_POINT('Ctrl Pts',(1.69623414782771,1.,1.03384646003588));
#24390=CARTESIAN_POINT('Ctrl Pts',(1.69231840863458,1.,1.02919977579147));
#24391=CARTESIAN_POINT('Ctrl Pts',(1.68836910178447,1.,1.02460180535255));
#24392=CARTESIAN_POINT('Ctrl Pts',(1.68440578021706,1.,1.02006795074201));
#24393=CARTESIAN_POINT('Ctrl Pts',(1.68044289894798,1.,1.01561026162773));
#24394=CARTESIAN_POINT('Ctrl Pts',(1.67648246776464,1.,1.01123236493511));
#24395=CARTESIAN_POINT('Ctrl Pts',(1.67250335383293,1.,1.00692206696414));
#24396=CARTESIAN_POINT('Ctrl Pts',(1.66846059277303,1.,1.00265091003727));
#24397=CARTESIAN_POINT('Ctrl Pts',(1.66430758030376,1.,0.998389654952758));
#24398=CARTESIAN_POINT('Ctrl Pts',(1.66001553809947,1.,0.994121836661306));
#24399=CARTESIAN_POINT('Ctrl Pts',(1.65559044289699,1.,0.989855627854165));
#24400=CARTESIAN_POINT('Ctrl Pts',(1.65110016612638,1.,0.985642622920821));
#24401=CARTESIAN_POINT('Ctrl Pts',(1.64665139190656,1.,0.981562530939489));
#24402=CARTESIAN_POINT('Ctrl Pts',(1.64233990826687,1.,0.977689794119417));
#24403=CARTESIAN_POINT('Ctrl Pts',(1.63820952658144,1.,0.974066058287419));
#24404=CARTESIAN_POINT('Ctrl Pts',(1.63420665729798,1.,0.970669715997509));
#24405=CARTESIAN_POINT('Ctrl Pts',(1.63013849959461,1.,0.967387853230345));
#24406=CARTESIAN_POINT('Ctrl Pts',(1.62571930670187,1.,0.964046107040536));
#24407=CARTESIAN_POINT('Ctrl Pts',(1.62061638140221,1.,0.960438326101729));
#24408=CARTESIAN_POINT('Ctrl Pts',(1.61449324337085,1.,0.956354422920671));
#24409=CARTESIAN_POINT('Ctrl Pts',(1.60706069896936,1.,0.951613284356035));
#24410=CARTESIAN_POINT('Ctrl Pts',(1.59810042043673,1.,0.946078063315257));
#24411=CARTESIAN_POINT('Ctrl Pts',(1.58744937487176,1.,0.939646377893399));
#24412=CARTESIAN_POINT('Ctrl Pts',(1.57499388382243,1.,0.932246680108685));
#24413=CARTESIAN_POINT('Ctrl Pts',(1.56065988578893,1.,0.923832188944341));
#24414=CARTESIAN_POINT('Ctrl Pts',(1.54440491149498,1.,0.914375919026456));
#24415=CARTESIAN_POINT('Ctrl Pts',(1.52984849887993,1.,0.905967409625651));
#24416=CARTESIAN_POINT('Ctrl Pts',(1.51805569590094,1.,0.899185047483511));
#24417=CARTESIAN_POINT('Ctrl Pts',(1.50980486806688,1.,0.894452006964544));
#24418=CARTESIAN_POINT('Ctrl Pts',(1.5055822144029,1.,0.892032620296856));
#24419=CARTESIAN_POINT('',(1.81978687191668,0.,1.23627494547115));
#24420=CARTESIAN_POINT('Origin',(1.73811241238545,0.,1.34869019493419));
#24421=CARTESIAN_POINT('',(1.73811241238545,1.,1.34869019493419));
#24422=CARTESIAN_POINT('',(1.81978687191668,1.,1.23627494547115));
#24423=CARTESIAN_POINT('',(1.73811241238545,0.,1.34869019493419));
#24424=CARTESIAN_POINT('Ctrl Pts',(1.31362392696032,-1.,1.15624053661742));
#24425=CARTESIAN_POINT('Ctrl Pts',(1.31362392696032,1.,1.15624053661742));
#24426=CARTESIAN_POINT('Ctrl Pts',(1.31722977216397,-1.,1.15950888730809));
#24427=CARTESIAN_POINT('Ctrl Pts',(1.31722977216397,1.,1.15950888730809));
#24428=CARTESIAN_POINT('Ctrl Pts',(1.32428080721772,-1.,1.16589330093588));
#24429=CARTESIAN_POINT('Ctrl Pts',(1.32428080721772,1.,1.16589330093588));
#24430=CARTESIAN_POINT('Ctrl Pts',(1.33437539347008,-1.,1.17501305789857));
#24431=CARTESIAN_POINT('Ctrl Pts',(1.33437539347008,1.,1.17501305789857));
#24432=CARTESIAN_POINT('Ctrl Pts',(1.34687054001093,-1.,1.18625865667441));
#24433=CARTESIAN_POINT('Ctrl Pts',(1.34687054001093,1.,1.18625865667441));
#24434=CARTESIAN_POINT('Ctrl Pts',(1.36088705043885,-1.,1.1987959077932));
#24435=CARTESIAN_POINT('Ctrl Pts',(1.36088705043885,1.,1.1987959077932));
#24436=CARTESIAN_POINT('Ctrl Pts',(1.37331915607905,-1.,1.20982812925645));
#24437=CARTESIAN_POINT('Ctrl Pts',(1.37331915607905,1.,1.20982812925645));
#24438=CARTESIAN_POINT('Ctrl Pts',(1.38420564527715,-1.,1.21938737280852));
#24439=CARTESIAN_POINT('Ctrl Pts',(1.38420564527715,1.,1.21938737280852));
#24440=CARTESIAN_POINT('Ctrl Pts',(1.39361389568796,-1.,1.22752961899387));
#24441=CARTESIAN_POINT('Ctrl Pts',(1.39361389568796,1.,1.22752961899387));
#24442=CARTESIAN_POINT('Ctrl Pts',(1.40164708206106,-1.,1.23434087290423));
#24443=CARTESIAN_POINT('Ctrl Pts',(1.40164708206106,1.,1.23434087290423));
#24444=CARTESIAN_POINT('Ctrl Pts',(1.40845295531283,-1.,1.23994455029534));
#24445=CARTESIAN_POINT('Ctrl Pts',(1.40845295531283,1.,1.23994455029534));
#24446=CARTESIAN_POINT('Ctrl Pts',(1.41422913175179,-1.,1.24450600513056));
#24447=CARTESIAN_POINT('Ctrl Pts',(1.41422913175179,1.,1.24450600513056));
#24448=CARTESIAN_POINT('Ctrl Pts',(1.41923722596025,-1.,1.24824430986571));
#24449=CARTESIAN_POINT('Ctrl Pts',(1.41923722596025,1.,1.24824430986571));
#24450=CARTESIAN_POINT('Ctrl Pts',(1.42378102115575,-1.,1.2514145557001));
#24451=CARTESIAN_POINT('Ctrl Pts',(1.42378102115575,1.,1.2514145557001));
#24452=CARTESIAN_POINT('Ctrl Pts',(1.42815938799387,-1.,1.25426945222639));
#24453=CARTESIAN_POINT('Ctrl Pts',(1.42815938799387,1.,1.25426945222639));
#24454=CARTESIAN_POINT('Ctrl Pts',(1.43262645609691,-1.,1.25702687965755));
#24455=CARTESIAN_POINT('Ctrl Pts',(1.43262645609691,1.,1.25702687965755));
#24456=CARTESIAN_POINT('Ctrl Pts',(1.43734919180847,-1.,1.25983531012005));
#24457=CARTESIAN_POINT('Ctrl Pts',(1.43734919180847,1.,1.25983531012005));
#24458=CARTESIAN_POINT('Ctrl Pts',(1.44236470511303,-1.,1.26273903323859));
#24459=CARTESIAN_POINT('Ctrl Pts',(1.44236470511303,1.,1.26273903323859));
#24460=CARTESIAN_POINT('Ctrl Pts',(1.44761985001662,-1.,1.26570925118868));
#24461=CARTESIAN_POINT('Ctrl Pts',(1.44761985001662,1.,1.26570925118868));
#24462=CARTESIAN_POINT('Ctrl Pts',(1.45301422764247,-1.,1.2686778680489));
#24463=CARTESIAN_POINT('Ctrl Pts',(1.45301422764247,1.,1.2686778680489));
#24464=CARTESIAN_POINT('Ctrl Pts',(1.45843906294697,-1.,1.27156805265289));
#24465=CARTESIAN_POINT('Ctrl Pts',(1.45843906294697,1.,1.27156805265289));
#24466=CARTESIAN_POINT('Ctrl Pts',(1.46382431332476,-1.,1.27433119897822));
#24467=CARTESIAN_POINT('Ctrl Pts',(1.46382431332476,1.,1.27433119897822));
#24468=CARTESIAN_POINT('Ctrl Pts',(1.46916035917133,-1.,1.2769641483109));
#24469=CARTESIAN_POINT('Ctrl Pts',(1.46916035917133,1.,1.2769641483109));
#24470=CARTESIAN_POINT('Ctrl Pts',(1.4744717526707,-1.,1.2794891824849));
#24471=CARTESIAN_POINT('Ctrl Pts',(1.4744717526707,1.,1.2794891824849));
#24472=CARTESIAN_POINT('Ctrl Pts',(1.47980070347095,-1.,1.28194158939517));
#24473=CARTESIAN_POINT('Ctrl Pts',(1.47980070347095,1.,1.28194158939517));
#24474=CARTESIAN_POINT('Ctrl Pts',(1.4851881711891,-1.,1.28435533880201));
#24475=CARTESIAN_POINT('Ctrl Pts',(1.4851881711891,1.,1.28435533880201));
#24476=CARTESIAN_POINT('Ctrl Pts',(1.4906522831278,-1.,1.2867467611644));
#24477=CARTESIAN_POINT('Ctrl Pts',(1.4906522831278,1.,1.2867467611644));
#24478=CARTESIAN_POINT('Ctrl Pts',(1.49618896881754,-1.,1.28911506584254));
#24479=CARTESIAN_POINT('Ctrl Pts',(1.49618896881754,1.,1.28911506584254));
#24480=CARTESIAN_POINT('Ctrl Pts',(1.50178230149776,-1.,1.29145022885181));
#24481=CARTESIAN_POINT('Ctrl Pts',(1.50178230149776,1.,1.29145022885181));
#24482=CARTESIAN_POINT('Ctrl Pts',(1.50741159078365,-1.,1.29373841372842));
#24483=CARTESIAN_POINT('Ctrl Pts',(1.50741159078365,1.,1.29373841372842));
#24484=CARTESIAN_POINT('Ctrl Pts',(1.51305994241402,-1.,1.29596850710509));
#24485=CARTESIAN_POINT('Ctrl Pts',(1.51305994241402,1.,1.29596850710509));
#24486=CARTESIAN_POINT('Ctrl Pts',(1.51872184912724,-1.,1.29813791800747));
#24487=CARTESIAN_POINT('Ctrl Pts',(1.51872184912724,1.,1.29813791800747));
#24488=CARTESIAN_POINT('Ctrl Pts',(1.52439957861062,-1.,1.30024984366328));
#24489=CARTESIAN_POINT('Ctrl Pts',(1.52439957861062,1.,1.30024984366328));
#24490=CARTESIAN_POINT('Ctrl Pts',(1.53009970283891,-1.,1.30231064395568));
#24491=CARTESIAN_POINT('Ctrl Pts',(1.53009970283891,1.,1.30231064395568));
#24492=CARTESIAN_POINT('Ctrl Pts',(1.53582981268977,-1.,1.30432735639489));
#24493=CARTESIAN_POINT('Ctrl Pts',(1.53582981268977,1.,1.30432735639489));
#24494=CARTESIAN_POINT('Ctrl Pts',(1.54159462645432,-1.,1.30630475189556));
#24495=CARTESIAN_POINT('Ctrl Pts',(1.54159462645432,1.,1.30630475189556));
#24496=CARTESIAN_POINT('Ctrl Pts',(1.54739413957185,-1.,1.30824393907473));
#24497=CARTESIAN_POINT('Ctrl Pts',(1.54739413957185,1.,1.30824393907473));
#24498=CARTESIAN_POINT('Ctrl Pts',(1.55322568759481,-1.,1.31014393684222));
#24499=CARTESIAN_POINT('Ctrl Pts',(1.55322568759481,1.,1.31014393684222));
#24500=CARTESIAN_POINT('Ctrl Pts',(1.55908521254821,-1.,1.31200264341696));
#24501=CARTESIAN_POINT('Ctrl Pts',(1.55908521254821,1.,1.31200264341696));
#24502=CARTESIAN_POINT('Ctrl Pts',(1.56496872402353,-1.,1.31381795281002));
#24503=CARTESIAN_POINT('Ctrl Pts',(1.56496872402353,1.,1.31381795281002));
#24504=CARTESIAN_POINT('Ctrl Pts',(1.57087397835723,-1.,1.31558903860016));
#24505=CARTESIAN_POINT('Ctrl Pts',(1.57087397835723,1.,1.31558903860016));
#24506=CARTESIAN_POINT('Ctrl Pts',(1.5768005650559,-1.,1.31731642317187));
#24507=CARTESIAN_POINT('Ctrl Pts',(1.5768005650559,1.,1.31731642317187));
#24508=CARTESIAN_POINT('Ctrl Pts',(1.58274907898834,-1.,1.31900135021432));
#24509=CARTESIAN_POINT('Ctrl Pts',(1.58274907898834,1.,1.31900135021432));
#24510=CARTESIAN_POINT('Ctrl Pts',(1.58872057258245,-1.,1.32064537110892));
#24511=CARTESIAN_POINT('Ctrl Pts',(1.58872057258245,1.,1.32064537110892));
#24512=CARTESIAN_POINT('Ctrl Pts',(1.59471591079403,-1.,1.32224985747682));
#24513=CARTESIAN_POINT('Ctrl Pts',(1.59471591079403,1.,1.32224985747682));
#24514=CARTESIAN_POINT('Ctrl Pts',(1.60073511858687,-1.,1.32381550858256));
#24515=CARTESIAN_POINT('Ctrl Pts',(1.60073511858687,1.,1.32381550858256));
#24516=CARTESIAN_POINT('Ctrl Pts',(1.60677758290954,-1.,1.32534250785782));
#24517=CARTESIAN_POINT('Ctrl Pts',(1.60677758290954,1.,1.32534250785782));
#24518=CARTESIAN_POINT('Ctrl Pts',(1.6128423401575,-1.,1.32683074483356));
#24519=CARTESIAN_POINT('Ctrl Pts',(1.6128423401575,1.,1.32683074483356));
#24520=CARTESIAN_POINT('Ctrl Pts',(1.61892832270724,-1.,1.32828000610449));
#24521=CARTESIAN_POINT('Ctrl Pts',(1.61892832270724,1.,1.32828000610449));
#24522=CARTESIAN_POINT('Ctrl Pts',(1.62503464209797,-1.,1.3296901950568));
#24523=CARTESIAN_POINT('Ctrl Pts',(1.62503464209797,1.,1.3296901950568));
#24524=CARTESIAN_POINT('Ctrl Pts',(1.63116079730923,-1.,1.33106149345645));
#24525=CARTESIAN_POINT('Ctrl Pts',(1.63116079730923,1.,1.33106149345645));
#24526=CARTESIAN_POINT('Ctrl Pts',(1.63730653475089,-1.,1.33239425103724));
#24527=CARTESIAN_POINT('Ctrl Pts',(1.63730653475089,1.,1.33239425103724));
#24528=CARTESIAN_POINT('Ctrl Pts',(1.6434717485603,-1.,1.33368890676572));
#24529=CARTESIAN_POINT('Ctrl Pts',(1.6434717485603,1.,1.33368890676572));
#24530=CARTESIAN_POINT('Ctrl Pts',(1.6496563728683,-1.,1.33494590467993));
#24531=CARTESIAN_POINT('Ctrl Pts',(1.6496563728683,1.,1.33494590467993));
#24532=CARTESIAN_POINT('Ctrl Pts',(1.65586025952593,-1.,1.33616559745172));
#24533=CARTESIAN_POINT('Ctrl Pts',(1.65586025952593,1.,1.33616559745172));
#24534=CARTESIAN_POINT('Ctrl Pts',(1.66208312541983,-1.,1.33734820885262));
#24535=CARTESIAN_POINT('Ctrl Pts',(1.66208312541983,1.,1.33734820885262));
#24536=CARTESIAN_POINT('Ctrl Pts',(1.66832460783989,-1.,1.33849388654388));
#24537=CARTESIAN_POINT('Ctrl Pts',(1.66832460783989,1.,1.33849388654388));
#24538=CARTESIAN_POINT('Ctrl Pts',(1.67458429426086,-1.,1.3396027347034));
#24539=CARTESIAN_POINT('Ctrl Pts',(1.67458429426086,1.,1.3396027347034));
#24540=CARTESIAN_POINT('Ctrl Pts',(1.68086176030362,-1.,1.34067485185203));
#24541=CARTESIAN_POINT('Ctrl Pts',(1.68086176030362,1.,1.34067485185203));
#24542=CARTESIAN_POINT('Ctrl Pts',(1.68715660868764,-1.,1.341710374848));
#24543=CARTESIAN_POINT('Ctrl Pts',(1.68715660868764,1.,1.341710374848));
#24544=CARTESIAN_POINT('Ctrl Pts',(1.6934684849687,-1.,1.34270948206319));
#24545=CARTESIAN_POINT('Ctrl Pts',(1.6934684849687,1.,1.34270948206319));
#24546=CARTESIAN_POINT('Ctrl Pts',(1.69979707754427,-1.,1.34367237124483));
#24547=CARTESIAN_POINT('Ctrl Pts',(1.69979707754427,1.,1.34367237124483));
#24548=CARTESIAN_POINT('Ctrl Pts',(1.70614212266738,-1.,1.34459924533831));
#24549=CARTESIAN_POINT('Ctrl Pts',(1.70614212266738,1.,1.34459924533831));
#24550=CARTESIAN_POINT('Ctrl Pts',(1.71250340686822,-1.,1.34549029589416));
#24551=CARTESIAN_POINT('Ctrl Pts',(1.71250340686822,1.,1.34549029589416));
#24552=CARTESIAN_POINT('Ctrl Pts',(1.7188807715049,-1.,1.34634568653227));
#24553=CARTESIAN_POINT('Ctrl Pts',(1.7188807715049,1.,1.34634568653227));
#24554=CARTESIAN_POINT('Ctrl Pts',(1.72527410680674,-1.,1.34716554819527));
#24555=CARTESIAN_POINT('Ctrl Pts',(1.72527410680674,1.,1.34716554819527));
#24556=CARTESIAN_POINT('Ctrl Pts',(1.7304014965394,-1.,1.34779309152035));
#24557=CARTESIAN_POINT('Ctrl Pts',(1.7304014965394,1.,1.34779309152035));
#24558=CARTESIAN_POINT('Ctrl Pts',(1.73425417885907,-1.,1.34824783112887));
#24559=CARTESIAN_POINT('Ctrl Pts',(1.73425417885907,1.,1.34824783112887));
#24560=CARTESIAN_POINT('Ctrl Pts',(1.73682580585691,-1.,1.34854391898045));
#24561=CARTESIAN_POINT('Ctrl Pts',(1.73682580585691,1.,1.34854391898045));
#24562=CARTESIAN_POINT('Ctrl Pts',(1.73811241238545,-1.,1.34869019493419));
#24563=CARTESIAN_POINT('Ctrl Pts',(1.73811241238545,1.,1.34869019493419));
#24564=CARTESIAN_POINT('',(1.31362392696032,1.,1.15624053661742));
#24565=CARTESIAN_POINT('Ctrl Pts',(1.31362392696032,1.,1.15624053661742));
#24566=CARTESIAN_POINT('Ctrl Pts',(1.31722977216397,1.,1.15950888730809));
#24567=CARTESIAN_POINT('Ctrl Pts',(1.32428080721772,1.,1.16589330093588));
#24568=CARTESIAN_POINT('Ctrl Pts',(1.33437539347008,1.,1.17501305789857));
#24569=CARTESIAN_POINT('Ctrl Pts',(1.34687054001093,1.,1.18625865667441));
#24570=CARTESIAN_POINT('Ctrl Pts',(1.36088705043885,1.,1.1987959077932));
#24571=CARTESIAN_POINT('Ctrl Pts',(1.37331915607905,1.,1.20982812925645));
#24572=CARTESIAN_POINT('Ctrl Pts',(1.38420564527715,1.,1.21938737280852));
#24573=CARTESIAN_POINT('Ctrl Pts',(1.39361389568796,1.,1.22752961899387));
#24574=CARTESIAN_POINT('Ctrl Pts',(1.40164708206106,1.,1.23434087290423));
#24575=CARTESIAN_POINT('Ctrl Pts',(1.40845295531283,1.,1.23994455029534));
#24576=CARTESIAN_POINT('Ctrl Pts',(1.41422913175179,1.,1.24450600513056));
#24577=CARTESIAN_POINT('Ctrl Pts',(1.41923722596025,1.,1.24824430986571));
#24578=CARTESIAN_POINT('Ctrl Pts',(1.42378102115575,1.,1.2514145557001));
#24579=CARTESIAN_POINT('Ctrl Pts',(1.42815938799387,1.,1.25426945222639));
#24580=CARTESIAN_POINT('Ctrl Pts',(1.43262645609691,1.,1.25702687965755));
#24581=CARTESIAN_POINT('Ctrl Pts',(1.43734919180847,1.,1.25983531012005));
#24582=CARTESIAN_POINT('Ctrl Pts',(1.44236470511303,1.,1.26273903323859));
#24583=CARTESIAN_POINT('Ctrl Pts',(1.44761985001662,1.,1.26570925118868));
#24584=CARTESIAN_POINT('Ctrl Pts',(1.45301422764247,1.,1.2686778680489));
#24585=CARTESIAN_POINT('Ctrl Pts',(1.45843906294697,1.,1.27156805265289));
#24586=CARTESIAN_POINT('Ctrl Pts',(1.46382431332476,1.,1.27433119897822));
#24587=CARTESIAN_POINT('Ctrl Pts',(1.46916035917133,1.,1.2769641483109));
#24588=CARTESIAN_POINT('Ctrl Pts',(1.4744717526707,1.,1.2794891824849));
#24589=CARTESIAN_POINT('Ctrl Pts',(1.47980070347095,1.,1.28194158939517));
#24590=CARTESIAN_POINT('Ctrl Pts',(1.4851881711891,1.,1.28435533880201));
#24591=CARTESIAN_POINT('Ctrl Pts',(1.4906522831278,1.,1.2867467611644));
#24592=CARTESIAN_POINT('Ctrl Pts',(1.49618896881754,1.,1.28911506584254));
#24593=CARTESIAN_POINT('Ctrl Pts',(1.50178230149776,1.,1.29145022885181));
#24594=CARTESIAN_POINT('Ctrl Pts',(1.50741159078365,1.,1.29373841372842));
#24595=CARTESIAN_POINT('Ctrl Pts',(1.51305994241402,1.,1.29596850710509));
#24596=CARTESIAN_POINT('Ctrl Pts',(1.51872184912724,1.,1.29813791800747));
#24597=CARTESIAN_POINT('Ctrl Pts',(1.52439957861062,1.,1.30024984366328));
#24598=CARTESIAN_POINT('Ctrl Pts',(1.53009970283891,1.,1.30231064395568));
#24599=CARTESIAN_POINT('Ctrl Pts',(1.53582981268977,1.,1.30432735639489));
#24600=CARTESIAN_POINT('Ctrl Pts',(1.54159462645432,1.,1.30630475189556));
#24601=CARTESIAN_POINT('Ctrl Pts',(1.54739413957185,1.,1.30824393907473));
#24602=CARTESIAN_POINT('Ctrl Pts',(1.55322568759481,1.,1.31014393684222));
#24603=CARTESIAN_POINT('Ctrl Pts',(1.55908521254821,1.,1.31200264341696));
#24604=CARTESIAN_POINT('Ctrl Pts',(1.56496872402353,1.,1.31381795281002));
#24605=CARTESIAN_POINT('Ctrl Pts',(1.57087397835723,1.,1.31558903860016));
#24606=CARTESIAN_POINT('Ctrl Pts',(1.5768005650559,1.,1.31731642317187));
#24607=CARTESIAN_POINT('Ctrl Pts',(1.58274907898834,1.,1.31900135021432));
#24608=CARTESIAN_POINT('Ctrl Pts',(1.58872057258245,1.,1.32064537110892));
#24609=CARTESIAN_POINT('Ctrl Pts',(1.59471591079403,1.,1.32224985747682));
#24610=CARTESIAN_POINT('Ctrl Pts',(1.60073511858687,1.,1.32381550858256));
#24611=CARTESIAN_POINT('Ctrl Pts',(1.60677758290954,1.,1.32534250785782));
#24612=CARTESIAN_POINT('Ctrl Pts',(1.6128423401575,1.,1.32683074483356));
#24613=CARTESIAN_POINT('Ctrl Pts',(1.61892832270724,1.,1.32828000610449));
#24614=CARTESIAN_POINT('Ctrl Pts',(1.62503464209797,1.,1.3296901950568));
#24615=CARTESIAN_POINT('Ctrl Pts',(1.63116079730923,1.,1.33106149345645));
#24616=CARTESIAN_POINT('Ctrl Pts',(1.63730653475089,1.,1.33239425103724));
#24617=CARTESIAN_POINT('Ctrl Pts',(1.6434717485603,1.,1.33368890676572));
#24618=CARTESIAN_POINT('Ctrl Pts',(1.6496563728683,1.,1.33494590467993));
#24619=CARTESIAN_POINT('Ctrl Pts',(1.65586025952593,1.,1.33616559745172));
#24620=CARTESIAN_POINT('Ctrl Pts',(1.66208312541983,1.,1.33734820885262));
#24621=CARTESIAN_POINT('Ctrl Pts',(1.66832460783989,1.,1.33849388654388));
#24622=CARTESIAN_POINT('Ctrl Pts',(1.67458429426086,1.,1.3396027347034));
#24623=CARTESIAN_POINT('Ctrl Pts',(1.68086176030362,1.,1.34067485185203));
#24624=CARTESIAN_POINT('Ctrl Pts',(1.68715660868764,1.,1.341710374848));
#24625=CARTESIAN_POINT('Ctrl Pts',(1.6934684849687,1.,1.34270948206319));
#24626=CARTESIAN_POINT('Ctrl Pts',(1.69979707754427,1.,1.34367237124483));
#24627=CARTESIAN_POINT('Ctrl Pts',(1.70614212266738,1.,1.34459924533831));
#24628=CARTESIAN_POINT('Ctrl Pts',(1.71250340686822,1.,1.34549029589416));
#24629=CARTESIAN_POINT('Ctrl Pts',(1.7188807715049,1.,1.34634568653227));
#24630=CARTESIAN_POINT('Ctrl Pts',(1.72527410680674,1.,1.34716554819527));
#24631=CARTESIAN_POINT('Ctrl Pts',(1.7304014965394,1.,1.34779309152035));
#24632=CARTESIAN_POINT('Ctrl Pts',(1.73425417885907,1.,1.34824783112887));
#24633=CARTESIAN_POINT('Ctrl Pts',(1.73682580585691,1.,1.34854391898045));
#24634=CARTESIAN_POINT('Ctrl Pts',(1.73811241238545,1.,1.34869019493419));
#24635=CARTESIAN_POINT('',(1.31362392696032,0.,1.15624053661742));
#24636=CARTESIAN_POINT('Origin',(0.,0.,0.));
#24637=CARTESIAN_POINT('',(1.15624053661742,1.,1.31362392696033));
#24638=CARTESIAN_POINT('Origin',(0.,1.,0.));
#24639=CARTESIAN_POINT('',(1.15624053661742,0.,1.31362392696032));
#24640=CARTESIAN_POINT('Ctrl Pts',(1.34869019493419,-1.,1.73811241238545));
#24641=CARTESIAN_POINT('Ctrl Pts',(1.34869019493419,1.,1.73811241238545));
#24642=CARTESIAN_POINT('Ctrl Pts',(1.34854391898145,-1.,1.73682580585819));
#24643=CARTESIAN_POINT('Ctrl Pts',(1.34854391898145,1.,1.73682580585819));
#24644=CARTESIAN_POINT('Ctrl Pts',(1.34824783113158,-1.,1.73425417886255));
#24645=CARTESIAN_POINT('Ctrl Pts',(1.34824783113158,1.,1.73425417886255));
#24646=CARTESIAN_POINT('Ctrl Pts',(1.3477930915247,-1.,1.73040149654497));
#24647=CARTESIAN_POINT('Ctrl Pts',(1.3477930915247,1.,1.73040149654497));
#24648=CARTESIAN_POINT('Ctrl Pts',(1.34716554820013,-1.,1.72527410681298));
#24649=CARTESIAN_POINT('Ctrl Pts',(1.34716554820013,1.,1.72527410681298));
#24650=CARTESIAN_POINT('Ctrl Pts',(1.34634568653586,-1.,1.7188807715095));
#24651=CARTESIAN_POINT('Ctrl Pts',(1.34634568653586,1.,1.7188807715095));
#24652=CARTESIAN_POINT('Ctrl Pts',(1.34549029589563,-1.,1.71250340687011));
#24653=CARTESIAN_POINT('Ctrl Pts',(1.34549029589563,1.,1.71250340687011));
#24654=CARTESIAN_POINT('Ctrl Pts',(1.34459924533783,-1.,1.70614212266676));
#24655=CARTESIAN_POINT('Ctrl Pts',(1.34459924533783,1.,1.70614212266676));
#24656=CARTESIAN_POINT('Ctrl Pts',(1.34367237124322,-1.,1.69979707754221));
#24657=CARTESIAN_POINT('Ctrl Pts',(1.34367237124322,1.,1.69979707754221));
#24658=CARTESIAN_POINT('Ctrl Pts',(1.34270948206139,-1.,1.6934684849664));
#24659=CARTESIAN_POINT('Ctrl Pts',(1.34270948206139,1.,1.6934684849664));
#24660=CARTESIAN_POINT('Ctrl Pts',(1.34171037484673,-1.,1.68715660868602));
#24661=CARTESIAN_POINT('Ctrl Pts',(1.34171037484673,1.,1.68715660868602));
#24662=CARTESIAN_POINT('Ctrl Pts',(1.3406748518516,-1.,1.68086176030308));
#24663=CARTESIAN_POINT('Ctrl Pts',(1.3406748518516,1.,1.68086176030308));
#24664=CARTESIAN_POINT('Ctrl Pts',(1.33960273470372,-1.,1.67458429426126));
#24665=CARTESIAN_POINT('Ctrl Pts',(1.33960273470372,1.,1.67458429426126));
#24666=CARTESIAN_POINT('Ctrl Pts',(1.33849388654458,-1.,1.66832460784078));
#24667=CARTESIAN_POINT('Ctrl Pts',(1.33849388654458,1.,1.66832460784078));
#24668=CARTESIAN_POINT('Ctrl Pts',(1.33734820885331,-1.,1.66208312542073));
#24669=CARTESIAN_POINT('Ctrl Pts',(1.33734820885331,1.,1.66208312542073));
#24670=CARTESIAN_POINT('Ctrl Pts',(1.33616559745217,-1.,1.65586025952651));
#24671=CARTESIAN_POINT('Ctrl Pts',(1.33616559745217,1.,1.65586025952651));
#24672=CARTESIAN_POINT('Ctrl Pts',(1.33494590468003,-1.,1.64965637286843));
#24673=CARTESIAN_POINT('Ctrl Pts',(1.33494590468003,1.,1.64965637286843));
#24674=CARTESIAN_POINT('Ctrl Pts',(1.33368890676554,-1.,1.64347174856007));
#24675=CARTESIAN_POINT('Ctrl Pts',(1.33368890676554,1.,1.64347174856007));
#24676=CARTESIAN_POINT('Ctrl Pts',(1.33239425103694,-1.,1.6373065347505));
#24677=CARTESIAN_POINT('Ctrl Pts',(1.33239425103694,1.,1.6373065347505));
#24678=CARTESIAN_POINT('Ctrl Pts',(1.33106149345618,-1.,1.63116079730887));
#24679=CARTESIAN_POINT('Ctrl Pts',(1.33106149345618,1.,1.63116079730887));
#24680=CARTESIAN_POINT('Ctrl Pts',(1.32969019505665,-1.,1.62503464209777));
#24681=CARTESIAN_POINT('Ctrl Pts',(1.32969019505665,1.,1.62503464209777));
#24682=CARTESIAN_POINT('Ctrl Pts',(1.32828000610448,-1.,1.61892832270723));
#24683=CARTESIAN_POINT('Ctrl Pts',(1.32828000610448,1.,1.61892832270723));
#24684=CARTESIAN_POINT('Ctrl Pts',(1.32683074483365,-1.,1.61284234015762));
#24685=CARTESIAN_POINT('Ctrl Pts',(1.32683074483365,1.,1.61284234015762));
#24686=CARTESIAN_POINT('Ctrl Pts',(1.32534250785794,-1.,1.6067775829097));
#24687=CARTESIAN_POINT('Ctrl Pts',(1.32534250785794,1.,1.6067775829097));
#24688=CARTESIAN_POINT('Ctrl Pts',(1.32381550858266,-1.,1.600735118587));
#24689=CARTESIAN_POINT('Ctrl Pts',(1.32381550858266,1.,1.600735118587));
#24690=CARTESIAN_POINT('Ctrl Pts',(1.32224985747686,-1.,1.59471591079408));
#24691=CARTESIAN_POINT('Ctrl Pts',(1.32224985747686,1.,1.59471591079408));
#24692=CARTESIAN_POINT('Ctrl Pts',(1.32064537110891,-1.,1.58872057258244));
#24693=CARTESIAN_POINT('Ctrl Pts',(1.32064537110891,1.,1.58872057258244));
#24694=CARTESIAN_POINT('Ctrl Pts',(1.31900135021428,-1.,1.58274907898829));
#24695=CARTESIAN_POINT('Ctrl Pts',(1.31900135021428,1.,1.58274907898829));
#24696=CARTESIAN_POINT('Ctrl Pts',(1.31731642317183,-1.,1.57680056505585));
#24697=CARTESIAN_POINT('Ctrl Pts',(1.31731642317183,1.,1.57680056505585));
#24698=CARTESIAN_POINT('Ctrl Pts',(1.31558903860015,-1.,1.57087397835721));
#24699=CARTESIAN_POINT('Ctrl Pts',(1.31558903860015,1.,1.57087397835721));
#24700=CARTESIAN_POINT('Ctrl Pts',(1.31381795281002,-1.,1.56496872402352));
#24701=CARTESIAN_POINT('Ctrl Pts',(1.31381795281002,1.,1.56496872402352));
#24702=CARTESIAN_POINT('Ctrl Pts',(1.31200264341696,-1.,1.55908521254822));
#24703=CARTESIAN_POINT('Ctrl Pts',(1.31200264341696,1.,1.55908521254822));
#24704=CARTESIAN_POINT('Ctrl Pts',(1.31014393684221,-1.,1.55322568759481));
#24705=CARTESIAN_POINT('Ctrl Pts',(1.31014393684221,1.,1.55322568759481));
#24706=CARTESIAN_POINT('Ctrl Pts',(1.30824393907471,-1.,1.54739413957183));
#24707=CARTESIAN_POINT('Ctrl Pts',(1.30824393907471,1.,1.54739413957183));
#24708=CARTESIAN_POINT('Ctrl Pts',(1.30630475189553,-1.,1.54159462645428));
#24709=CARTESIAN_POINT('Ctrl Pts',(1.30630475189553,1.,1.54159462645428));
#24710=CARTESIAN_POINT('Ctrl Pts',(1.30432735639487,-1.,1.53582981268976));
#24711=CARTESIAN_POINT('Ctrl Pts',(1.30432735639487,1.,1.53582981268976));
#24712=CARTESIAN_POINT('Ctrl Pts',(1.3023106439557,-1.,1.53009970283893));
#24713=CARTESIAN_POINT('Ctrl Pts',(1.3023106439557,1.,1.53009970283893));
#24714=CARTESIAN_POINT('Ctrl Pts',(1.30024984366334,-1.,1.5243995786107));
#24715=CARTESIAN_POINT('Ctrl Pts',(1.30024984366334,1.,1.5243995786107));
#24716=CARTESIAN_POINT('Ctrl Pts',(1.29813791800757,-1.,1.51872184912735));
#24717=CARTESIAN_POINT('Ctrl Pts',(1.29813791800757,1.,1.51872184912735));
#24718=CARTESIAN_POINT('Ctrl Pts',(1.29596850710518,-1.,1.51305994241412));
#24719=CARTESIAN_POINT('Ctrl Pts',(1.29596850710518,1.,1.51305994241412));
#24720=CARTESIAN_POINT('Ctrl Pts',(1.29373841372843,-1.,1.50741159078367));
#24721=CARTESIAN_POINT('Ctrl Pts',(1.29373841372843,1.,1.50741159078367));
#24722=CARTESIAN_POINT('Ctrl Pts',(1.29145022885171,-1.,1.50178230149764));
#24723=CARTESIAN_POINT('Ctrl Pts',(1.29145022885171,1.,1.50178230149764));
#24724=CARTESIAN_POINT('Ctrl Pts',(1.28911506584232,-1.,1.49618896881729));
#24725=CARTESIAN_POINT('Ctrl Pts',(1.28911506584232,1.,1.49618896881729));
#24726=CARTESIAN_POINT('Ctrl Pts',(1.28674676116415,-1.,1.4906522831275));
#24727=CARTESIAN_POINT('Ctrl Pts',(1.28674676116415,1.,1.4906522831275));
#24728=CARTESIAN_POINT('Ctrl Pts',(1.28435533880184,-1.,1.48518817118891));
#24729=CARTESIAN_POINT('Ctrl Pts',(1.28435533880184,1.,1.48518817118891));
#24730=CARTESIAN_POINT('Ctrl Pts',(1.28194158939522,-1.,1.47980070347102));
#24731=CARTESIAN_POINT('Ctrl Pts',(1.28194158939522,1.,1.47980070347102));
#24732=CARTESIAN_POINT('Ctrl Pts',(1.27948918248524,-1.,1.4744717526711));
#24733=CARTESIAN_POINT('Ctrl Pts',(1.27948918248524,1.,1.4744717526711));
#24734=CARTESIAN_POINT('Ctrl Pts',(1.27696414831144,-1.,1.46916035917197));
#24735=CARTESIAN_POINT('Ctrl Pts',(1.27696414831144,1.,1.46916035917197));
#24736=CARTESIAN_POINT('Ctrl Pts',(1.27433119897877,-1.,1.4638243133254));
#24737=CARTESIAN_POINT('Ctrl Pts',(1.27433119897877,1.,1.4638243133254));
#24738=CARTESIAN_POINT('Ctrl Pts',(1.27156805265312,-1.,1.45843906294725));
#24739=CARTESIAN_POINT('Ctrl Pts',(1.27156805265312,1.,1.45843906294725));
#24740=CARTESIAN_POINT('Ctrl Pts',(1.26867786804854,-1.,1.45301422764205));
#24741=CARTESIAN_POINT('Ctrl Pts',(1.26867786804854,1.,1.45301422764205));
#24742=CARTESIAN_POINT('Ctrl Pts',(1.26570925118767,-1.,1.44761985001544));
#24743=CARTESIAN_POINT('Ctrl Pts',(1.26570925118767,1.,1.44761985001544));
#24744=CARTESIAN_POINT('Ctrl Pts',(1.26273903323723,-1.,1.44236470511145));
#24745=CARTESIAN_POINT('Ctrl Pts',(1.26273903323723,1.,1.44236470511145));
#24746=CARTESIAN_POINT('Ctrl Pts',(1.25983531011894,-1.,1.43734919180719));
#24747=CARTESIAN_POINT('Ctrl Pts',(1.25983531011894,1.,1.43734919180719));
#24748=CARTESIAN_POINT('Ctrl Pts',(1.25702687965744,-1.,1.43262645609679));
#24749=CARTESIAN_POINT('Ctrl Pts',(1.25702687965744,1.,1.43262645609679));
#24750=CARTESIAN_POINT('Ctrl Pts',(1.25426945222783,-1.,1.42815938799555));
#24751=CARTESIAN_POINT('Ctrl Pts',(1.25426945222783,1.,1.42815938799555));
#24752=CARTESIAN_POINT('Ctrl Pts',(1.25141455570299,-1.,1.42378102115911));
#24753=CARTESIAN_POINT('Ctrl Pts',(1.25141455570299,1.,1.42378102115911));
#24754=CARTESIAN_POINT('Ctrl Pts',(1.24824430986911,-1.,1.41923722596421));
#24755=CARTESIAN_POINT('Ctrl Pts',(1.24824430986911,1.,1.41923722596421));
#24756=CARTESIAN_POINT('Ctrl Pts',(1.24450600513278,-1.,1.41422913175437));
#24757=CARTESIAN_POINT('Ctrl Pts',(1.24450600513278,1.,1.41422913175437));
#24758=CARTESIAN_POINT('Ctrl Pts',(1.23994455029421,-1.,1.40845295531151));
#24759=CARTESIAN_POINT('Ctrl Pts',(1.23994455029421,1.,1.40845295531151));
#24760=CARTESIAN_POINT('Ctrl Pts',(1.23434087289768,-1.,1.40164708205345));
#24761=CARTESIAN_POINT('Ctrl Pts',(1.23434087289768,1.,1.40164708205345));
#24762=CARTESIAN_POINT('Ctrl Pts',(1.22752961898063,-1.,1.39361389567257));
#24763=CARTESIAN_POINT('Ctrl Pts',(1.22752961898063,1.,1.39361389567257));
#24764=CARTESIAN_POINT('Ctrl Pts',(1.21938737278853,-1.,1.38420564525391));
#24765=CARTESIAN_POINT('Ctrl Pts',(1.21938737278853,1.,1.38420564525391));
#24766=CARTESIAN_POINT('Ctrl Pts',(1.20982812923113,-1.,1.37331915604962));
#24767=CARTESIAN_POINT('Ctrl Pts',(1.20982812923113,1.,1.37331915604962));
#24768=CARTESIAN_POINT('Ctrl Pts',(1.1987959077656,-1.,1.36088705040677));
#24769=CARTESIAN_POINT('Ctrl Pts',(1.1987959077656,1.,1.36088705040677));
#24770=CARTESIAN_POINT('Ctrl Pts',(1.18625865664915,-1.,1.34687053998157));
#24771=CARTESIAN_POINT('Ctrl Pts',(1.18625865664915,1.,1.34687053998157));
#24772=CARTESIAN_POINT('Ctrl Pts',(1.17501305787994,-1.,1.33437539344842));
#24773=CARTESIAN_POINT('Ctrl Pts',(1.17501305787994,1.,1.33437539344842));
#24774=CARTESIAN_POINT('Ctrl Pts',(1.16589330092532,-1.,1.32428080720544));
#24775=CARTESIAN_POINT('Ctrl Pts',(1.16589330092532,1.,1.32428080720544));
#24776=CARTESIAN_POINT('Ctrl Pts',(1.15950888730433,-1.,1.3172297721596));
#24777=CARTESIAN_POINT('Ctrl Pts',(1.15950888730433,1.,1.3172297721596));
#24778=CARTESIAN_POINT('Ctrl Pts',(1.15624053661742,-1.,1.31362392696033));
#24779=CARTESIAN_POINT('Ctrl Pts',(1.15624053661742,1.,1.31362392696033));
#24780=CARTESIAN_POINT('',(1.34869019493419,1.,1.73811241238545));
#24781=CARTESIAN_POINT('Ctrl Pts',(1.34869019493419,1.,1.73811241238545));
#24782=CARTESIAN_POINT('Ctrl Pts',(1.34854391898145,1.,1.73682580585819));
#24783=CARTESIAN_POINT('Ctrl Pts',(1.34824783113158,1.,1.73425417886255));
#24784=CARTESIAN_POINT('Ctrl Pts',(1.3477930915247,1.,1.73040149654497));
#24785=CARTESIAN_POINT('Ctrl Pts',(1.34716554820013,1.,1.72527410681298));
#24786=CARTESIAN_POINT('Ctrl Pts',(1.34634568653586,1.,1.7188807715095));
#24787=CARTESIAN_POINT('Ctrl Pts',(1.34549029589563,1.,1.71250340687011));
#24788=CARTESIAN_POINT('Ctrl Pts',(1.34459924533783,1.,1.70614212266676));
#24789=CARTESIAN_POINT('Ctrl Pts',(1.34367237124322,1.,1.69979707754221));
#24790=CARTESIAN_POINT('Ctrl Pts',(1.34270948206139,1.,1.6934684849664));
#24791=CARTESIAN_POINT('Ctrl Pts',(1.34171037484673,1.,1.68715660868602));
#24792=CARTESIAN_POINT('Ctrl Pts',(1.3406748518516,1.,1.68086176030308));
#24793=CARTESIAN_POINT('Ctrl Pts',(1.33960273470372,1.,1.67458429426126));
#24794=CARTESIAN_POINT('Ctrl Pts',(1.33849388654458,1.,1.66832460784078));
#24795=CARTESIAN_POINT('Ctrl Pts',(1.33734820885331,1.,1.66208312542073));
#24796=CARTESIAN_POINT('Ctrl Pts',(1.33616559745217,1.,1.65586025952651));
#24797=CARTESIAN_POINT('Ctrl Pts',(1.33494590468003,1.,1.64965637286843));
#24798=CARTESIAN_POINT('Ctrl Pts',(1.33368890676554,1.,1.64347174856007));
#24799=CARTESIAN_POINT('Ctrl Pts',(1.33239425103694,1.,1.6373065347505));
#24800=CARTESIAN_POINT('Ctrl Pts',(1.33106149345618,1.,1.63116079730887));
#24801=CARTESIAN_POINT('Ctrl Pts',(1.32969019505665,1.,1.62503464209777));
#24802=CARTESIAN_POINT('Ctrl Pts',(1.32828000610448,1.,1.61892832270723));
#24803=CARTESIAN_POINT('Ctrl Pts',(1.32683074483365,1.,1.61284234015762));
#24804=CARTESIAN_POINT('Ctrl Pts',(1.32534250785794,1.,1.6067775829097));
#24805=CARTESIAN_POINT('Ctrl Pts',(1.32381550858266,1.,1.600735118587));
#24806=CARTESIAN_POINT('Ctrl Pts',(1.32224985747686,1.,1.59471591079408));
#24807=CARTESIAN_POINT('Ctrl Pts',(1.32064537110891,1.,1.58872057258244));
#24808=CARTESIAN_POINT('Ctrl Pts',(1.31900135021428,1.,1.58274907898829));
#24809=CARTESIAN_POINT('Ctrl Pts',(1.31731642317183,1.,1.57680056505585));
#24810=CARTESIAN_POINT('Ctrl Pts',(1.31558903860015,1.,1.57087397835721));
#24811=CARTESIAN_POINT('Ctrl Pts',(1.31381795281002,1.,1.56496872402352));
#24812=CARTESIAN_POINT('Ctrl Pts',(1.31200264341696,1.,1.55908521254822));
#24813=CARTESIAN_POINT('Ctrl Pts',(1.31014393684221,1.,1.55322568759481));
#24814=CARTESIAN_POINT('Ctrl Pts',(1.30824393907471,1.,1.54739413957183));
#24815=CARTESIAN_POINT('Ctrl Pts',(1.30630475189553,1.,1.54159462645428));
#24816=CARTESIAN_POINT('Ctrl Pts',(1.30432735639487,1.,1.53582981268976));
#24817=CARTESIAN_POINT('Ctrl Pts',(1.3023106439557,1.,1.53009970283893));
#24818=CARTESIAN_POINT('Ctrl Pts',(1.30024984366334,1.,1.5243995786107));
#24819=CARTESIAN_POINT('Ctrl Pts',(1.29813791800757,1.,1.51872184912735));
#24820=CARTESIAN_POINT('Ctrl Pts',(1.29596850710518,1.,1.51305994241412));
#24821=CARTESIAN_POINT('Ctrl Pts',(1.29373841372843,1.,1.50741159078367));
#24822=CARTESIAN_POINT('Ctrl Pts',(1.29145022885171,1.,1.50178230149764));
#24823=CARTESIAN_POINT('Ctrl Pts',(1.28911506584232,1.,1.49618896881729));
#24824=CARTESIAN_POINT('Ctrl Pts',(1.28674676116415,1.,1.4906522831275));
#24825=CARTESIAN_POINT('Ctrl Pts',(1.28435533880184,1.,1.48518817118891));
#24826=CARTESIAN_POINT('Ctrl Pts',(1.28194158939522,1.,1.47980070347102));
#24827=CARTESIAN_POINT('Ctrl Pts',(1.27948918248524,1.,1.4744717526711));
#24828=CARTESIAN_POINT('Ctrl Pts',(1.27696414831144,1.,1.46916035917197));
#24829=CARTESIAN_POINT('Ctrl Pts',(1.27433119897877,1.,1.4638243133254));
#24830=CARTESIAN_POINT('Ctrl Pts',(1.27156805265312,1.,1.45843906294725));
#24831=CARTESIAN_POINT('Ctrl Pts',(1.26867786804854,1.,1.45301422764205));
#24832=CARTESIAN_POINT('Ctrl Pts',(1.26570925118767,1.,1.44761985001544));
#24833=CARTESIAN_POINT('Ctrl Pts',(1.26273903323723,1.,1.44236470511145));
#24834=CARTESIAN_POINT('Ctrl Pts',(1.25983531011894,1.,1.43734919180719));
#24835=CARTESIAN_POINT('Ctrl Pts',(1.25702687965744,1.,1.43262645609679));
#24836=CARTESIAN_POINT('Ctrl Pts',(1.25426945222783,1.,1.42815938799555));
#24837=CARTESIAN_POINT('Ctrl Pts',(1.25141455570299,1.,1.42378102115911));
#24838=CARTESIAN_POINT('Ctrl Pts',(1.24824430986911,1.,1.41923722596421));
#24839=CARTESIAN_POINT('Ctrl Pts',(1.24450600513278,1.,1.41422913175437));
#24840=CARTESIAN_POINT('Ctrl Pts',(1.23994455029421,1.,1.40845295531151));
#24841=CARTESIAN_POINT('Ctrl Pts',(1.23434087289768,1.,1.40164708205345));
#24842=CARTESIAN_POINT('Ctrl Pts',(1.22752961898063,1.,1.39361389567257));
#24843=CARTESIAN_POINT('Ctrl Pts',(1.21938737278853,1.,1.38420564525391));
#24844=CARTESIAN_POINT('Ctrl Pts',(1.20982812923113,1.,1.37331915604962));
#24845=CARTESIAN_POINT('Ctrl Pts',(1.1987959077656,1.,1.36088705040677));
#24846=CARTESIAN_POINT('Ctrl Pts',(1.18625865664915,1.,1.34687053998157));
#24847=CARTESIAN_POINT('Ctrl Pts',(1.17501305787994,1.,1.33437539344842));
#24848=CARTESIAN_POINT('Ctrl Pts',(1.16589330092532,1.,1.32428080720544));
#24849=CARTESIAN_POINT('Ctrl Pts',(1.15950888730433,1.,1.3172297721596));
#24850=CARTESIAN_POINT('Ctrl Pts',(1.15624053661742,1.,1.31362392696033));
#24851=CARTESIAN_POINT('',(1.34869019493419,0.,1.73811241238545));
#24852=CARTESIAN_POINT('Origin',(1.23627494547115,0.,1.81978687191668));
#24853=CARTESIAN_POINT('',(1.23627494547115,1.,1.81978687191668));
#24854=CARTESIAN_POINT('',(1.34869019493419,1.,1.73811241238545));
#24855=CARTESIAN_POINT('',(1.23627494547115,0.,1.81978687191668));
#24856=CARTESIAN_POINT('Ctrl Pts',(0.892032620296855,-1.,1.5055822144029));
#24857=CARTESIAN_POINT('Ctrl Pts',(0.892032620296855,1.,1.5055822144029));
#24858=CARTESIAN_POINT('Ctrl Pts',(0.894452006967538,-1.,1.50980486807181));
#24859=CARTESIAN_POINT('Ctrl Pts',(0.894452006967538,1.,1.50980486807181));
#24860=CARTESIAN_POINT('Ctrl Pts',(0.89918504749193,-1.,1.51805569591479));
#24861=CARTESIAN_POINT('Ctrl Pts',(0.89918504749193,1.,1.51805569591479));
#24862=CARTESIAN_POINT('Ctrl Pts',(0.905967409640498,-1.,1.52984849890434));
#24863=CARTESIAN_POINT('Ctrl Pts',(0.905967409640498,1.,1.52984849890434));
#24864=CARTESIAN_POINT('Ctrl Pts',(0.914375919046579,-1.,1.54440491152808));
#24865=CARTESIAN_POINT('Ctrl Pts',(0.914375919046579,1.,1.54440491152808));
#24866=CARTESIAN_POINT('Ctrl Pts',(0.923832188966322,-1.,1.56065988582509));
#24867=CARTESIAN_POINT('Ctrl Pts',(0.923832188966322,1.,1.56065988582509));
#24868=CARTESIAN_POINT('Ctrl Pts',(0.932246680128848,-1.,1.57499388385561));
#24869=CARTESIAN_POINT('Ctrl Pts',(0.932246680128848,1.,1.57499388385561));
#24870=CARTESIAN_POINT('Ctrl Pts',(0.939646377909319,-1.,1.58744937489796));
#24871=CARTESIAN_POINT('Ctrl Pts',(0.939646377909319,1.,1.58744937489796));
#24872=CARTESIAN_POINT('Ctrl Pts',(0.946078063325795,-1.,1.59810042045408));
#24873=CARTESIAN_POINT('Ctrl Pts',(0.946078063325795,1.,1.59810042045408));
#24874=CARTESIAN_POINT('Ctrl Pts',(0.951613284361247,-1.,1.60706069897794));
#24875=CARTESIAN_POINT('Ctrl Pts',(0.951613284361247,1.,1.60706069897794));
#24876=CARTESIAN_POINT('Ctrl Pts',(0.956354422921572,-1.,1.61449324337233));
#24877=CARTESIAN_POINT('Ctrl Pts',(0.956354422921572,1.,1.61449324337233));
#24878=CARTESIAN_POINT('Ctrl Pts',(0.960438326099958,-1.,1.62061638139929));
#24879=CARTESIAN_POINT('Ctrl Pts',(0.960438326099958,1.,1.62061638139929));
#24880=CARTESIAN_POINT('Ctrl Pts',(0.964046107037821,-1.,1.6257193066974));
#24881=CARTESIAN_POINT('Ctrl Pts',(0.964046107037821,1.,1.6257193066974));
#24882=CARTESIAN_POINT('Ctrl Pts',(0.967387853228041,-1.,1.63013849959083));
#24883=CARTESIAN_POINT('Ctrl Pts',(0.967387853228041,1.,1.63013849959083));
#24884=CARTESIAN_POINT('Ctrl Pts',(0.970669715996356,-1.,1.63420665729609));
#24885=CARTESIAN_POINT('Ctrl Pts',(0.970669715996356,1.,1.63420665729609));
#24886=CARTESIAN_POINT('Ctrl Pts',(0.974066058287501,-1.,1.63820952658157));
#24887=CARTESIAN_POINT('Ctrl Pts',(0.974066058287501,1.,1.63820952658157));
#24888=CARTESIAN_POINT('Ctrl Pts',(0.977689794120296,-1.,1.64233990826831));
#24889=CARTESIAN_POINT('Ctrl Pts',(0.977689794120296,1.,1.64233990826831));
#24890=CARTESIAN_POINT('Ctrl Pts',(0.981562530940574,-1.,1.64665139190834));
#24891=CARTESIAN_POINT('Ctrl Pts',(0.981562530940574,1.,1.64665139190834));
#24892=CARTESIAN_POINT('Ctrl Pts',(0.985642622921626,-1.,1.6511001661277));
#24893=CARTESIAN_POINT('Ctrl Pts',(0.985642622921626,1.,1.6511001661277));
#24894=CARTESIAN_POINT('Ctrl Pts',(0.98985562785445,-1.,1.65559044289746));
#24895=CARTESIAN_POINT('Ctrl Pts',(0.98985562785445,1.,1.65559044289746));
#24896=CARTESIAN_POINT('Ctrl Pts',(0.994121836661115,-1.,1.66001553809916));
#24897=CARTESIAN_POINT('Ctrl Pts',(0.994121836661115,1.,1.66001553809916));
#24898=CARTESIAN_POINT('Ctrl Pts',(0.998389654952317,-1.,1.66430758030304));
#24899=CARTESIAN_POINT('Ctrl Pts',(0.998389654952317,1.,1.66430758030304));
#24900=CARTESIAN_POINT('Ctrl Pts',(1.00265091003682,-1.,1.66846059277231));
#24901=CARTESIAN_POINT('Ctrl Pts',(1.00265091003682,1.,1.66846059277231));
#24902=CARTESIAN_POINT('Ctrl Pts',(1.00692206696387,-1.,1.67250335383248));
#24903=CARTESIAN_POINT('Ctrl Pts',(1.00692206696387,1.,1.67250335383248));
#24904=CARTESIAN_POINT('Ctrl Pts',(1.01123236493507,-1.,1.67648246776457));
#24905=CARTESIAN_POINT('Ctrl Pts',(1.01123236493507,1.,1.67648246776457));
#24906=CARTESIAN_POINT('Ctrl Pts',(1.01561026162786,-1.,1.6804428989482));
#24907=CARTESIAN_POINT('Ctrl Pts',(1.01561026162786,1.,1.6804428989482));
#24908=CARTESIAN_POINT('Ctrl Pts',(1.02006795074222,-1.,1.68440578021739));
#24909=CARTESIAN_POINT('Ctrl Pts',(1.02006795074222,1.,1.68440578021739));
#24910=CARTESIAN_POINT('Ctrl Pts',(1.02460180535272,-1.,1.68836910178475));
#24911=CARTESIAN_POINT('Ctrl Pts',(1.02460180535272,1.,1.68836910178475));
#24912=CARTESIAN_POINT('Ctrl Pts',(1.02919977579155,-1.,1.69231840863471));
#24913=CARTESIAN_POINT('Ctrl Pts',(1.02919977579155,1.,1.69231840863471));
#24914=CARTESIAN_POINT('Ctrl Pts',(1.03384646003587,-1.,1.69623414782769));
#24915=CARTESIAN_POINT('Ctrl Pts',(1.03384646003587,1.,1.69623414782769));
#24916=CARTESIAN_POINT('Ctrl Pts',(1.03852922490782,-1.,1.70010052930951));
#24917=CARTESIAN_POINT('Ctrl Pts',(1.03852922490782,1.,1.70010052930951));
#24918=CARTESIAN_POINT('Ctrl Pts',(1.04324363334546,-1.,1.70391338707969));
#24919=CARTESIAN_POINT('Ctrl Pts',(1.04324363334546,1.,1.70391338707969));
#24920=CARTESIAN_POINT('Ctrl Pts',(1.0479908540499,-1.,1.70767646263641));
#24921=CARTESIAN_POINT('Ctrl Pts',(1.0479908540499,1.,1.70767646263641));
#24922=CARTESIAN_POINT('Ctrl Pts',(1.05277517202853,-1.,1.71139783543986));
#24923=CARTESIAN_POINT('Ctrl Pts',(1.05277517202853,1.,1.71139783543986));
#24924=CARTESIAN_POINT('Ctrl Pts',(1.05760163192481,-1.,1.71508654427022));
#24925=CARTESIAN_POINT('Ctrl Pts',(1.05760163192481,1.,1.71508654427022));
#24926=CARTESIAN_POINT('Ctrl Pts',(1.06247324680649,-1.,1.71874858456908));
#24927=CARTESIAN_POINT('Ctrl Pts',(1.06247324680649,1.,1.71874858456908));
#24928=CARTESIAN_POINT('Ctrl Pts',(1.06738966975463,-1.,1.72238500928456));
#24929=CARTESIAN_POINT('Ctrl Pts',(1.06738966975463,1.,1.72238500928456));
#24930=CARTESIAN_POINT('Ctrl Pts',(1.07234866990252,-1.,1.72599406198489));
#24931=CARTESIAN_POINT('Ctrl Pts',(1.07234866990252,1.,1.72599406198489));
#24932=CARTESIAN_POINT('Ctrl Pts',(1.0773470373727,-1.,1.72957248977424));
#24933=CARTESIAN_POINT('Ctrl Pts',(1.0773470373727,1.,1.72957248977424));
#24934=CARTESIAN_POINT('Ctrl Pts',(1.08238162784749,-1.,1.73311705663407));
#24935=CARTESIAN_POINT('Ctrl Pts',(1.08238162784749,1.,1.73311705663407));
#24936=CARTESIAN_POINT('Ctrl Pts',(1.08745056285429,-1.,1.73662628326093));
#24937=CARTESIAN_POINT('Ctrl Pts',(1.08745056285429,1.,1.73662628326093));
#24938=CARTESIAN_POINT('Ctrl Pts',(1.09255329056496,-1.,1.74010053962252));
#24939=CARTESIAN_POINT('Ctrl Pts',(1.09255329056496,1.,1.74010053962252));
#24940=CARTESIAN_POINT('Ctrl Pts',(1.09768999241229,-1.,1.74354119236212));
#24941=CARTESIAN_POINT('Ctrl Pts',(1.09768999241229,1.,1.74354119236212));
#24942=CARTESIAN_POINT('Ctrl Pts',(1.10286118991144,-1.,1.74695004214924));
#24943=CARTESIAN_POINT('Ctrl Pts',(1.10286118991144,1.,1.74695004214924));
#24944=CARTESIAN_POINT('Ctrl Pts',(1.10806728183003,-1.,1.75032866075914));
#24945=CARTESIAN_POINT('Ctrl Pts',(1.10806728183003,1.,1.75032866075914));
#24946=CARTESIAN_POINT('Ctrl Pts',(1.11330807582542,-1.,1.75367772094617));
#24947=CARTESIAN_POINT('Ctrl Pts',(1.11330807582542,1.,1.75367772094617));
#24948=CARTESIAN_POINT('Ctrl Pts',(1.11858293216752,-1.,1.75699720772089));
#24949=CARTESIAN_POINT('Ctrl Pts',(1.11858293216752,1.,1.75699720772089));
#24950=CARTESIAN_POINT('Ctrl Pts',(1.12389096855078,-1.,1.76028671825084));
#24951=CARTESIAN_POINT('Ctrl Pts',(1.12389096855078,1.,1.76028671825084));
#24952=CARTESIAN_POINT('Ctrl Pts',(1.12923123555076,-1.,1.76354571966171));
#24953=CARTESIAN_POINT('Ctrl Pts',(1.12923123555076,1.,1.76354571966171));
#24954=CARTESIAN_POINT('Ctrl Pts',(1.13460291804634,-1.,1.76677384551883));
#24955=CARTESIAN_POINT('Ctrl Pts',(1.13460291804634,1.,1.76677384551883));
#24956=CARTESIAN_POINT('Ctrl Pts',(1.14000548337,-1.,1.76997111386806));
#24957=CARTESIAN_POINT('Ctrl Pts',(1.14000548337,1.,1.76997111386806));
#24958=CARTESIAN_POINT('Ctrl Pts',(1.14543858226948,-1.,1.77313777896234));
#24959=CARTESIAN_POINT('Ctrl Pts',(1.14543858226948,1.,1.77313777896234));
#24960=CARTESIAN_POINT('Ctrl Pts',(1.15090197841531,-1.,1.77627422557034));
#24961=CARTESIAN_POINT('Ctrl Pts',(1.15090197841531,1.,1.77627422557034));
#24962=CARTESIAN_POINT('Ctrl Pts',(1.15639547194689,-1.,1.77938085564261));
#24963=CARTESIAN_POINT('Ctrl Pts',(1.15639547194689,1.,1.77938085564261));
#24964=CARTESIAN_POINT('Ctrl Pts',(1.16191881298458,-1.,1.78245795880949));
#24965=CARTESIAN_POINT('Ctrl Pts',(1.16191881298458,1.,1.78245795880949));
#24966=CARTESIAN_POINT('Ctrl Pts',(1.16747166312239,-1.,1.78550566040349));
#24967=CARTESIAN_POINT('Ctrl Pts',(1.16747166312239,1.,1.78550566040349));
#24968=CARTESIAN_POINT('Ctrl Pts',(1.17305363177265,-1.,1.78852398877523));
#24969=CARTESIAN_POINT('Ctrl Pts',(1.17305363177265,1.,1.78852398877523));
#24970=CARTESIAN_POINT('Ctrl Pts',(1.17866429440781,-1.,1.79151291552646));
#24971=CARTESIAN_POINT('Ctrl Pts',(1.17866429440781,1.,1.79151291552646));
#24972=CARTESIAN_POINT('Ctrl Pts',(1.18430321697471,-1.,1.79447240321572));
#24973=CARTESIAN_POINT('Ctrl Pts',(1.18430321697471,1.,1.79447240321572));
#24974=CARTESIAN_POINT('Ctrl Pts',(1.1899699793456,-1.,1.79740245923649));
#24975=CARTESIAN_POINT('Ctrl Pts',(1.1899699793456,1.,1.79740245923649));
#24976=CARTESIAN_POINT('Ctrl Pts',(1.19566418930405,-1.,1.80030314370121));
#24977=CARTESIAN_POINT('Ctrl Pts',(1.19566418930405,1.,1.80030314370121));
#24978=CARTESIAN_POINT('Ctrl Pts',(1.2013854893912,-1.,1.8031745483882));
#24979=CARTESIAN_POINT('Ctrl Pts',(1.2013854893912,1.,1.8031745483882));
#24980=CARTESIAN_POINT('Ctrl Pts',(1.20713356605519,-1.,1.80601678480772));
#24981=CARTESIAN_POINT('Ctrl Pts',(1.20713356605519,1.,1.80601678480772));
#24982=CARTESIAN_POINT('Ctrl Pts',(1.2129081570818,-1.,1.80882996916931));
#24983=CARTESIAN_POINT('Ctrl Pts',(1.2129081570818,1.,1.80882996916931));
#24984=CARTESIAN_POINT('Ctrl Pts',(1.2187090610323,-1.,1.81161420806172));
#24985=CARTESIAN_POINT('Ctrl Pts',(1.2187090610323,1.,1.81161420806172));
#24986=CARTESIAN_POINT('Ctrl Pts',(1.22453613304507,-1.,1.81436959209778));
#24987=CARTESIAN_POINT('Ctrl Pts',(1.22453613304507,1.,1.81436959209778));
#24988=CARTESIAN_POINT('Ctrl Pts',(1.22921864890975,-1.,1.81655087183054));
#24989=CARTESIAN_POINT('Ctrl Pts',(1.22921864890975,1.,1.81655087183054));
#24990=CARTESIAN_POINT('Ctrl Pts',(1.23274224526804,-1.,1.81817389920914));
#24991=CARTESIAN_POINT('Ctrl Pts',(1.23274224526804,1.,1.81817389920914));
#24992=CARTESIAN_POINT('Ctrl Pts',(1.23509651170384,-1.,1.81925017193531));
#24993=CARTESIAN_POINT('Ctrl Pts',(1.23509651170384,1.,1.81925017193531));
#24994=CARTESIAN_POINT('Ctrl Pts',(1.23627494547115,-1.,1.81978687191668));
#24995=CARTESIAN_POINT('Ctrl Pts',(1.23627494547115,1.,1.81978687191668));
#24996=CARTESIAN_POINT('',(0.892032620296855,1.,1.5055822144029));
#24997=CARTESIAN_POINT('Ctrl Pts',(0.892032620296855,1.,1.5055822144029));
#24998=CARTESIAN_POINT('Ctrl Pts',(0.894452006967538,1.,1.50980486807181));
#24999=CARTESIAN_POINT('Ctrl Pts',(0.89918504749193,1.,1.51805569591479));
#25000=CARTESIAN_POINT('Ctrl Pts',(0.905967409640498,1.,1.52984849890434));
#25001=CARTESIAN_POINT('Ctrl Pts',(0.914375919046579,1.,1.54440491152808));
#25002=CARTESIAN_POINT('Ctrl Pts',(0.923832188966322,1.,1.56065988582509));
#25003=CARTESIAN_POINT('Ctrl Pts',(0.932246680128848,1.,1.57499388385561));
#25004=CARTESIAN_POINT('Ctrl Pts',(0.939646377909319,1.,1.58744937489796));
#25005=CARTESIAN_POINT('Ctrl Pts',(0.946078063325795,1.,1.59810042045408));
#25006=CARTESIAN_POINT('Ctrl Pts',(0.951613284361247,1.,1.60706069897794));
#25007=CARTESIAN_POINT('Ctrl Pts',(0.956354422921572,1.,1.61449324337233));
#25008=CARTESIAN_POINT('Ctrl Pts',(0.960438326099958,1.,1.62061638139929));
#25009=CARTESIAN_POINT('Ctrl Pts',(0.964046107037821,1.,1.6257193066974));
#25010=CARTESIAN_POINT('Ctrl Pts',(0.967387853228041,1.,1.63013849959083));
#25011=CARTESIAN_POINT('Ctrl Pts',(0.970669715996356,1.,1.63420665729609));
#25012=CARTESIAN_POINT('Ctrl Pts',(0.974066058287501,1.,1.63820952658157));
#25013=CARTESIAN_POINT('Ctrl Pts',(0.977689794120296,1.,1.64233990826831));
#25014=CARTESIAN_POINT('Ctrl Pts',(0.981562530940574,1.,1.64665139190834));
#25015=CARTESIAN_POINT('Ctrl Pts',(0.985642622921626,1.,1.6511001661277));
#25016=CARTESIAN_POINT('Ctrl Pts',(0.98985562785445,1.,1.65559044289746));
#25017=CARTESIAN_POINT('Ctrl Pts',(0.994121836661115,1.,1.66001553809916));
#25018=CARTESIAN_POINT('Ctrl Pts',(0.998389654952317,1.,1.66430758030304));
#25019=CARTESIAN_POINT('Ctrl Pts',(1.00265091003682,1.,1.66846059277231));
#25020=CARTESIAN_POINT('Ctrl Pts',(1.00692206696387,1.,1.67250335383248));
#25021=CARTESIAN_POINT('Ctrl Pts',(1.01123236493507,1.,1.67648246776457));
#25022=CARTESIAN_POINT('Ctrl Pts',(1.01561026162786,1.,1.6804428989482));
#25023=CARTESIAN_POINT('Ctrl Pts',(1.02006795074222,1.,1.68440578021739));
#25024=CARTESIAN_POINT('Ctrl Pts',(1.02460180535272,1.,1.68836910178475));
#25025=CARTESIAN_POINT('Ctrl Pts',(1.02919977579155,1.,1.69231840863471));
#25026=CARTESIAN_POINT('Ctrl Pts',(1.03384646003587,1.,1.69623414782769));
#25027=CARTESIAN_POINT('Ctrl Pts',(1.03852922490782,1.,1.70010052930951));
#25028=CARTESIAN_POINT('Ctrl Pts',(1.04324363334546,1.,1.70391338707969));
#25029=CARTESIAN_POINT('Ctrl Pts',(1.0479908540499,1.,1.70767646263641));
#25030=CARTESIAN_POINT('Ctrl Pts',(1.05277517202853,1.,1.71139783543986));
#25031=CARTESIAN_POINT('Ctrl Pts',(1.05760163192481,1.,1.71508654427022));
#25032=CARTESIAN_POINT('Ctrl Pts',(1.06247324680649,1.,1.71874858456908));
#25033=CARTESIAN_POINT('Ctrl Pts',(1.06738966975463,1.,1.72238500928456));
#25034=CARTESIAN_POINT('Ctrl Pts',(1.07234866990252,1.,1.72599406198489));
#25035=CARTESIAN_POINT('Ctrl Pts',(1.0773470373727,1.,1.72957248977424));
#25036=CARTESIAN_POINT('Ctrl Pts',(1.08238162784749,1.,1.73311705663407));
#25037=CARTESIAN_POINT('Ctrl Pts',(1.08745056285429,1.,1.73662628326093));
#25038=CARTESIAN_POINT('Ctrl Pts',(1.09255329056496,1.,1.74010053962252));
#25039=CARTESIAN_POINT('Ctrl Pts',(1.09768999241229,1.,1.74354119236212));
#25040=CARTESIAN_POINT('Ctrl Pts',(1.10286118991144,1.,1.74695004214924));
#25041=CARTESIAN_POINT('Ctrl Pts',(1.10806728183003,1.,1.75032866075914));
#25042=CARTESIAN_POINT('Ctrl Pts',(1.11330807582542,1.,1.75367772094617));
#25043=CARTESIAN_POINT('Ctrl Pts',(1.11858293216752,1.,1.75699720772089));
#25044=CARTESIAN_POINT('Ctrl Pts',(1.12389096855078,1.,1.76028671825084));
#25045=CARTESIAN_POINT('Ctrl Pts',(1.12923123555076,1.,1.76354571966171));
#25046=CARTESIAN_POINT('Ctrl Pts',(1.13460291804634,1.,1.76677384551883));
#25047=CARTESIAN_POINT('Ctrl Pts',(1.14000548337,1.,1.76997111386806));
#25048=CARTESIAN_POINT('Ctrl Pts',(1.14543858226948,1.,1.77313777896234));
#25049=CARTESIAN_POINT('Ctrl Pts',(1.15090197841531,1.,1.77627422557034));
#25050=CARTESIAN_POINT('Ctrl Pts',(1.15639547194689,1.,1.77938085564261));
#25051=CARTESIAN_POINT('Ctrl Pts',(1.16191881298458,1.,1.78245795880949));
#25052=CARTESIAN_POINT('Ctrl Pts',(1.16747166312239,1.,1.78550566040349));
#25053=CARTESIAN_POINT('Ctrl Pts',(1.17305363177265,1.,1.78852398877523));
#25054=CARTESIAN_POINT('Ctrl Pts',(1.17866429440781,1.,1.79151291552646));
#25055=CARTESIAN_POINT('Ctrl Pts',(1.18430321697471,1.,1.79447240321572));
#25056=CARTESIAN_POINT('Ctrl Pts',(1.1899699793456,1.,1.79740245923649));
#25057=CARTESIAN_POINT('Ctrl Pts',(1.19566418930405,1.,1.80030314370121));
#25058=CARTESIAN_POINT('Ctrl Pts',(1.2013854893912,1.,1.8031745483882));
#25059=CARTESIAN_POINT('Ctrl Pts',(1.20713356605519,1.,1.80601678480772));
#25060=CARTESIAN_POINT('Ctrl Pts',(1.2129081570818,1.,1.80882996916931));
#25061=CARTESIAN_POINT('Ctrl Pts',(1.2187090610323,1.,1.81161420806172));
#25062=CARTESIAN_POINT('Ctrl Pts',(1.22453613304507,1.,1.81436959209778));
#25063=CARTESIAN_POINT('Ctrl Pts',(1.22921864890975,1.,1.81655087183054));
#25064=CARTESIAN_POINT('Ctrl Pts',(1.23274224526804,1.,1.81817389920914));
#25065=CARTESIAN_POINT('Ctrl Pts',(1.23509651170384,1.,1.81925017193531));
#25066=CARTESIAN_POINT('Ctrl Pts',(1.23627494547115,1.,1.81978687191668));
#25067=CARTESIAN_POINT('',(0.892032620296854,0.,1.5055822144029));
#25068=CARTESIAN_POINT('Origin',(0.,0.,0.));
#25069=CARTESIAN_POINT('',(0.693717979106305,1.,1.60662857109684));
#25070=CARTESIAN_POINT('Origin',(0.,1.,0.));
#25071=CARTESIAN_POINT('',(0.693717979106305,0.,1.60662857109684));
#25072=CARTESIAN_POINT('Ctrl Pts',(0.7455743247944,-1.,2.0698113262342));
#25073=CARTESIAN_POINT('Ctrl Pts',(0.7455743247944,1.,2.0698113262342));
#25074=CARTESIAN_POINT('Ctrl Pts',(0.745832791378367,-1.,2.06854248895728));
#25075=CARTESIAN_POINT('Ctrl Pts',(0.745832791378367,1.,2.06854248895728));
#25076=CARTESIAN_POINT('Ctrl Pts',(0.7463458715442,-1.,2.06600523016815));
#25077=CARTESIAN_POINT('Ctrl Pts',(0.7463458715442,1.,2.06600523016815));
#25078=CARTESIAN_POINT('Ctrl Pts',(0.747103932787919,-1.,2.06220058927826));
#25079=CARTESIAN_POINT('Ctrl Pts',(0.747103932787919,1.,2.06220058927826));
#25080=CARTESIAN_POINT('Ctrl Pts',(0.748091554183802,-1.,2.05713023031007));
#25081=CARTESIAN_POINT('Ctrl Pts',(0.748091554183802,1.,2.05713023031007));
#25082=CARTESIAN_POINT('Ctrl Pts',(0.749287468665046,-1.,2.05079645592154));
#25083=CARTESIAN_POINT('Ctrl Pts',(0.749287468665046,1.,2.05079645592154));
#25084=CARTESIAN_POINT('Ctrl Pts',(0.750444657875575,-1.,2.04446689147979));
#25085=CARTESIAN_POINT('Ctrl Pts',(0.750444657875575,1.,2.04446689147979));
#25086=CARTESIAN_POINT('Ctrl Pts',(0.751562963361115,-1.,2.03814160092099));
#25087=CARTESIAN_POINT('Ctrl Pts',(0.751562963361115,1.,2.03814160092099));
#25088=CARTESIAN_POINT('Ctrl Pts',(0.75264218048721,-1.,2.03182068456221));
#25089=CARTESIAN_POINT('Ctrl Pts',(0.75264218048721,1.,2.03182068456221));
#25090=CARTESIAN_POINT('Ctrl Pts',(0.753682061112768,-1.,2.02550428623313));
#25091=CARTESIAN_POINT('Ctrl Pts',(0.753682061112768,1.,2.02550428623313));
#25092=CARTESIAN_POINT('Ctrl Pts',(0.754682330722816,-1.,2.01919259405809));
#25093=CARTESIAN_POINT('Ctrl Pts',(0.754682330722816,1.,2.01919259405809));
#25094=CARTESIAN_POINT('Ctrl Pts',(0.755642704957865,-1.,2.01288584328084));
#25095=CARTESIAN_POINT('Ctrl Pts',(0.755642704957865,1.,2.01288584328084));
#25096=CARTESIAN_POINT('Ctrl Pts',(0.75656290464667,-1.,2.0065843158773));
#25097=CARTESIAN_POINT('Ctrl Pts',(0.75656290464667,1.,2.0065843158773));
#25098=CARTESIAN_POINT('Ctrl Pts',(0.757442676862724,-1.,2.00028834739178));
#25099=CARTESIAN_POINT('Ctrl Pts',(0.757442676862724,1.,2.00028834739178));
#25100=CARTESIAN_POINT('Ctrl Pts',(0.758281796766761,-1.,1.99399831098817));
#25101=CARTESIAN_POINT('Ctrl Pts',(0.758281796766761,1.,1.99399831098817));
#25102=CARTESIAN_POINT('Ctrl Pts',(0.759080037802488,-1.,1.98771456680874));
#25103=CARTESIAN_POINT('Ctrl Pts',(0.759080037802488,1.,1.98771456680874));
#25104=CARTESIAN_POINT('Ctrl Pts',(0.75983714745219,-1.,1.98143741418172));
#25105=CARTESIAN_POINT('Ctrl Pts',(0.75983714745219,1.,1.98143741418172));
#25106=CARTESIAN_POINT('Ctrl Pts',(0.760552825409757,-1.,1.97516705321494));
#25107=CARTESIAN_POINT('Ctrl Pts',(0.760552825409757,1.,1.97516705321494));
#25108=CARTESIAN_POINT('Ctrl Pts',(0.76122669048382,-1.,1.96890351582499));
#25109=CARTESIAN_POINT('Ctrl Pts',(0.76122669048382,1.,1.96890351582499));
#25110=CARTESIAN_POINT('Ctrl Pts',(0.761858300014423,-1.,1.96264672744186));
#25111=CARTESIAN_POINT('Ctrl Pts',(0.761858300014423,1.,1.96264672744186));
#25112=CARTESIAN_POINT('Ctrl Pts',(0.762447203806178,-1.,1.95639665309869));
#25113=CARTESIAN_POINT('Ctrl Pts',(0.762447203806178,1.,1.95639665309869));
#25114=CARTESIAN_POINT('Ctrl Pts',(0.762992990878769,-1.,1.95015342590024));
#25115=CARTESIAN_POINT('Ctrl Pts',(0.762992990878769,1.,1.95015342590024));
#25116=CARTESIAN_POINT('Ctrl Pts',(0.763495333538629,-1.,1.9439174661764));
#25117=CARTESIAN_POINT('Ctrl Pts',(0.763495333538629,1.,1.9439174661764));
#25118=CARTESIAN_POINT('Ctrl Pts',(0.763954049121458,-1.,1.93768964875886));
#25119=CARTESIAN_POINT('Ctrl Pts',(0.763954049121458,1.,1.93768964875886));
#25120=CARTESIAN_POINT('Ctrl Pts',(0.76436901067394,-1.,1.93147105496382));
#25121=CARTESIAN_POINT('Ctrl Pts',(0.76436901067394,1.,1.93147105496382));
#25122=CARTESIAN_POINT('Ctrl Pts',(0.764740025488211,-1.,1.92526263537048));
#25123=CARTESIAN_POINT('Ctrl Pts',(0.764740025488211,1.,1.92526263537048));
#25124=CARTESIAN_POINT('Ctrl Pts',(0.765066729667088,-1.,1.91906491634196));
#25125=CARTESIAN_POINT('Ctrl Pts',(0.765066729667088,1.,1.91906491634196));
#25126=CARTESIAN_POINT('Ctrl Pts',(0.765348465884722,-1.,1.91287765805169));
#25127=CARTESIAN_POINT('Ctrl Pts',(0.765348465884722,1.,1.91287765805169));
#25128=CARTESIAN_POINT('Ctrl Pts',(0.765584196937919,-1.,1.90669961402356));
#25129=CARTESIAN_POINT('Ctrl Pts',(0.765584196937919,1.,1.90669961402356));
#25130=CARTESIAN_POINT('Ctrl Pts',(0.765772772593386,-1.,1.90052930393596));
#25131=CARTESIAN_POINT('Ctrl Pts',(0.765772772593386,1.,1.90052930393596));
#25132=CARTESIAN_POINT('Ctrl Pts',(0.765913193856978,-1.,1.89436577771388));
#25133=CARTESIAN_POINT('Ctrl Pts',(0.765913193856978,1.,1.89436577771388));
#25134=CARTESIAN_POINT('Ctrl Pts',(0.766004837062091,-1.,1.88820926433409));
#25135=CARTESIAN_POINT('Ctrl Pts',(0.766004837062091,1.,1.88820926433409));
#25136=CARTESIAN_POINT('Ctrl Pts',(0.766047794851864,-1.,1.88206215302561));
#25137=CARTESIAN_POINT('Ctrl Pts',(0.766047794851864,1.,1.88206215302561));
#25138=CARTESIAN_POINT('Ctrl Pts',(0.766042837036744,-1.,1.87592888967883));
#25139=CARTESIAN_POINT('Ctrl Pts',(0.766042837036744,1.,1.87592888967883));
#25140=CARTESIAN_POINT('Ctrl Pts',(0.765990708546091,-1.,1.86981398314341));
#25141=CARTESIAN_POINT('Ctrl Pts',(0.765990708546091,1.,1.86981398314341));
#25142=CARTESIAN_POINT('Ctrl Pts',(0.765891519092547,-1.,1.86372027063312));
#25143=CARTESIAN_POINT('Ctrl Pts',(0.765891519092547,1.,1.86372027063312));
#25144=CARTESIAN_POINT('Ctrl Pts',(0.765744212909318,-1.,1.85764741390394));
#25145=CARTESIAN_POINT('Ctrl Pts',(0.765744212909318,1.,1.85764741390394));
#25146=CARTESIAN_POINT('Ctrl Pts',(0.765545710619062,-1.,1.85158945130063));
#25147=CARTESIAN_POINT('Ctrl Pts',(0.765545710619062,1.,1.85158945130063));
#25148=CARTESIAN_POINT('Ctrl Pts',(0.765291664862029,-1.,1.84553698875924));
#25149=CARTESIAN_POINT('Ctrl Pts',(0.765291664862029,1.,1.84553698875924));
#25150=CARTESIAN_POINT('Ctrl Pts',(0.764978057881737,-1.,1.83948181064835));
#25151=CARTESIAN_POINT('Ctrl Pts',(0.764978057881737,1.,1.83948181064835));
#25152=CARTESIAN_POINT('Ctrl Pts',(0.764602549687853,-1.,1.83342077227142));
#25153=CARTESIAN_POINT('Ctrl Pts',(0.764602549687853,1.,1.83342077227142));
#25154=CARTESIAN_POINT('Ctrl Pts',(0.764165902605995,-1.,1.82735991200065));
#25155=CARTESIAN_POINT('Ctrl Pts',(0.764165902605995,1.,1.82735991200065));
#25156=CARTESIAN_POINT('Ctrl Pts',(0.763673465462726,-1.,1.82131873145266));
#25157=CARTESIAN_POINT('Ctrl Pts',(0.763673465462726,1.,1.82131873145266));
#25158=CARTESIAN_POINT('Ctrl Pts',(0.763132003836634,-1.,1.8153211840553));
#25159=CARTESIAN_POINT('Ctrl Pts',(0.763132003836634,1.,1.8153211840553));
#25160=CARTESIAN_POINT('Ctrl Pts',(0.762546129463938,-1.,1.80938551463965));
#25161=CARTESIAN_POINT('Ctrl Pts',(0.762546129463938,1.,1.80938551463965));
#25162=CARTESIAN_POINT('Ctrl Pts',(0.761915336443547,-1.,1.80351583877342));
#25163=CARTESIAN_POINT('Ctrl Pts',(0.761915336443547,1.,1.80351583877342));
#25164=CARTESIAN_POINT('Ctrl Pts',(0.761229695230558,-1.,1.79768986997783));
#25165=CARTESIAN_POINT('Ctrl Pts',(0.761229695230558,1.,1.79768986997783));
#25166=CARTESIAN_POINT('Ctrl Pts',(0.760469555880749,-1.,1.7918581561088));
#25167=CARTESIAN_POINT('Ctrl Pts',(0.760469555880749,1.,1.7918581561088));
#25168=CARTESIAN_POINT('Ctrl Pts',(0.759614401110189,-1.,1.78596964884604));
#25169=CARTESIAN_POINT('Ctrl Pts',(0.759614401110189,1.,1.78596964884604));
#25170=CARTESIAN_POINT('Ctrl Pts',(0.758650626677518,-1.,1.77999411220945));
#25171=CARTESIAN_POINT('Ctrl Pts',(0.758650626677518,1.,1.77999411220945));
#25172=CARTESIAN_POINT('Ctrl Pts',(0.757578264077028,-1.,1.77394167108292));
#25173=CARTESIAN_POINT('Ctrl Pts',(0.757578264077028,1.,1.77394167108292));
#25174=CARTESIAN_POINT('Ctrl Pts',(0.75642189602781,-1.,1.76789396002998));
#25175=CARTESIAN_POINT('Ctrl Pts',(0.75642189602781,1.,1.76789396002998));
#25176=CARTESIAN_POINT('Ctrl Pts',(0.755220979974461,-1.,1.76197817240128));
#25177=CARTESIAN_POINT('Ctrl Pts',(0.755220979974461,1.,1.76197817240128));
#25178=CARTESIAN_POINT('Ctrl Pts',(0.754009254027828,-1.,1.75631083600019));
#25179=CARTESIAN_POINT('Ctrl Pts',(0.754009254027828,1.,1.75631083600019));
#25180=CARTESIAN_POINT('Ctrl Pts',(0.752797683531314,-1.,1.75095139468794));
#25181=CARTESIAN_POINT('Ctrl Pts',(0.752797683531314,1.,1.75095139468794));
#25182=CARTESIAN_POINT('Ctrl Pts',(0.751555614164482,-1.,1.74585086852502));
#25183=CARTESIAN_POINT('Ctrl Pts',(0.751555614164482,1.,1.74585086852502));
#25184=CARTESIAN_POINT('Ctrl Pts',(0.750193435981249,-1.,1.74080458267114));
#25185=CARTESIAN_POINT('Ctrl Pts',(0.750193435981249,1.,1.74080458267114));
#25186=CARTESIAN_POINT('Ctrl Pts',(0.74858246295687,-1.,1.7355035168033));
#25187=CARTESIAN_POINT('Ctrl Pts',(0.74858246295687,1.,1.7355035168033));
#25188=CARTESIAN_POINT('Ctrl Pts',(0.746574710097752,-1.,1.72958533647714));
#25189=CARTESIAN_POINT('Ctrl Pts',(0.746574710097752,1.,1.72958533647714));
#25190=CARTESIAN_POINT('Ctrl Pts',(0.744021445433093,-1.,1.72268229916769));
#25191=CARTESIAN_POINT('Ctrl Pts',(0.744021445433093,1.,1.72268229916769));
#25192=CARTESIAN_POINT('Ctrl Pts',(0.74079516202821,-1.,1.71447789751001));
#25193=CARTESIAN_POINT('Ctrl Pts',(0.74079516202821,1.,1.71447789751001));
#25194=CARTESIAN_POINT('Ctrl Pts',(0.736799665716932,-1.,1.70473309004249));
#25195=CARTESIAN_POINT('Ctrl Pts',(0.736799665716932,1.,1.70473309004249));
#25196=CARTESIAN_POINT('Ctrl Pts',(0.731963238685357,-1.,1.69326921972915));
#25197=CARTESIAN_POINT('Ctrl Pts',(0.731963238685357,1.,1.69326921972915));
#25198=CARTESIAN_POINT('Ctrl Pts',(0.726235967982445,-1.,1.67996158451922));
#25199=CARTESIAN_POINT('Ctrl Pts',(0.726235967982445,1.,1.67996158451922));
#25200=CARTESIAN_POINT('Ctrl Pts',(0.719585433787949,-1.,1.66472880551777));
#25201=CARTESIAN_POINT('Ctrl Pts',(0.719585433787949,1.,1.66472880551777));
#25202=CARTESIAN_POINT('Ctrl Pts',(0.711993139340447,-1.,1.64752408828442));
#25203=CARTESIAN_POINT('Ctrl Pts',(0.711993139340447,1.,1.64752408828442));
#25204=CARTESIAN_POINT('Ctrl Pts',(0.705159151977294,-1.,1.6321654166204));
#25205=CARTESIAN_POINT('Ctrl Pts',(0.705159151977294,1.,1.6321654166204));
#25206=CARTESIAN_POINT('Ctrl Pts',(0.699605146398836,-1.,1.61974673471117));
#25207=CARTESIAN_POINT('Ctrl Pts',(0.699605146398836,1.,1.61974673471117));
#25208=CARTESIAN_POINT('Ctrl Pts',(0.69571209787897,-1.,1.61106790957619));
#25209=CARTESIAN_POINT('Ctrl Pts',(0.69571209787897,1.,1.61106790957619));
#25210=CARTESIAN_POINT('Ctrl Pts',(0.693717979106305,-1.,1.60662857109684));
#25211=CARTESIAN_POINT('Ctrl Pts',(0.693717979106305,1.,1.60662857109684));
#25212=CARTESIAN_POINT('',(0.7455743247944,1.,2.0698113262342));
#25213=CARTESIAN_POINT('Ctrl Pts',(0.7455743247944,1.,2.0698113262342));
#25214=CARTESIAN_POINT('Ctrl Pts',(0.745832791378367,1.,2.06854248895728));
#25215=CARTESIAN_POINT('Ctrl Pts',(0.7463458715442,1.,2.06600523016815));
#25216=CARTESIAN_POINT('Ctrl Pts',(0.747103932787919,1.,2.06220058927826));
#25217=CARTESIAN_POINT('Ctrl Pts',(0.748091554183802,1.,2.05713023031007));
#25218=CARTESIAN_POINT('Ctrl Pts',(0.749287468665046,1.,2.05079645592154));
#25219=CARTESIAN_POINT('Ctrl Pts',(0.750444657875575,1.,2.04446689147979));
#25220=CARTESIAN_POINT('Ctrl Pts',(0.751562963361115,1.,2.03814160092099));
#25221=CARTESIAN_POINT('Ctrl Pts',(0.75264218048721,1.,2.03182068456221));
#25222=CARTESIAN_POINT('Ctrl Pts',(0.753682061112768,1.,2.02550428623313));
#25223=CARTESIAN_POINT('Ctrl Pts',(0.754682330722816,1.,2.01919259405809));
#25224=CARTESIAN_POINT('Ctrl Pts',(0.755642704957865,1.,2.01288584328084));
#25225=CARTESIAN_POINT('Ctrl Pts',(0.75656290464667,1.,2.0065843158773));
#25226=CARTESIAN_POINT('Ctrl Pts',(0.757442676862724,1.,2.00028834739178));
#25227=CARTESIAN_POINT('Ctrl Pts',(0.758281796766761,1.,1.99399831098817));
#25228=CARTESIAN_POINT('Ctrl Pts',(0.759080037802488,1.,1.98771456680874));
#25229=CARTESIAN_POINT('Ctrl Pts',(0.75983714745219,1.,1.98143741418172));
#25230=CARTESIAN_POINT('Ctrl Pts',(0.760552825409757,1.,1.97516705321494));
#25231=CARTESIAN_POINT('Ctrl Pts',(0.76122669048382,1.,1.96890351582499));
#25232=CARTESIAN_POINT('Ctrl Pts',(0.761858300014423,1.,1.96264672744186));
#25233=CARTESIAN_POINT('Ctrl Pts',(0.762447203806178,1.,1.95639665309869));
#25234=CARTESIAN_POINT('Ctrl Pts',(0.762992990878769,1.,1.95015342590024));
#25235=CARTESIAN_POINT('Ctrl Pts',(0.763495333538629,1.,1.9439174661764));
#25236=CARTESIAN_POINT('Ctrl Pts',(0.763954049121458,1.,1.93768964875886));
#25237=CARTESIAN_POINT('Ctrl Pts',(0.76436901067394,1.,1.93147105496382));
#25238=CARTESIAN_POINT('Ctrl Pts',(0.764740025488211,1.,1.92526263537048));
#25239=CARTESIAN_POINT('Ctrl Pts',(0.765066729667088,1.,1.91906491634196));
#25240=CARTESIAN_POINT('Ctrl Pts',(0.765348465884722,1.,1.91287765805169));
#25241=CARTESIAN_POINT('Ctrl Pts',(0.765584196937919,1.,1.90669961402356));
#25242=CARTESIAN_POINT('Ctrl Pts',(0.765772772593386,1.,1.90052930393596));
#25243=CARTESIAN_POINT('Ctrl Pts',(0.765913193856978,1.,1.89436577771388));
#25244=CARTESIAN_POINT('Ctrl Pts',(0.766004837062091,1.,1.88820926433409));
#25245=CARTESIAN_POINT('Ctrl Pts',(0.766047794851864,1.,1.88206215302561));
#25246=CARTESIAN_POINT('Ctrl Pts',(0.766042837036744,1.,1.87592888967883));
#25247=CARTESIAN_POINT('Ctrl Pts',(0.765990708546091,1.,1.86981398314341));
#25248=CARTESIAN_POINT('Ctrl Pts',(0.765891519092547,1.,1.86372027063312));
#25249=CARTESIAN_POINT('Ctrl Pts',(0.765744212909318,1.,1.85764741390394));
#25250=CARTESIAN_POINT('Ctrl Pts',(0.765545710619062,1.,1.85158945130063));
#25251=CARTESIAN_POINT('Ctrl Pts',(0.765291664862029,1.,1.84553698875924));
#25252=CARTESIAN_POINT('Ctrl Pts',(0.764978057881737,1.,1.83948181064835));
#25253=CARTESIAN_POINT('Ctrl Pts',(0.764602549687853,1.,1.83342077227142));
#25254=CARTESIAN_POINT('Ctrl Pts',(0.764165902605995,1.,1.82735991200065));
#25255=CARTESIAN_POINT('Ctrl Pts',(0.763673465462726,1.,1.82131873145266));
#25256=CARTESIAN_POINT('Ctrl Pts',(0.763132003836634,1.,1.8153211840553));
#25257=CARTESIAN_POINT('Ctrl Pts',(0.762546129463938,1.,1.80938551463965));
#25258=CARTESIAN_POINT('Ctrl Pts',(0.761915336443547,1.,1.80351583877342));
#25259=CARTESIAN_POINT('Ctrl Pts',(0.761229695230558,1.,1.79768986997783));
#25260=CARTESIAN_POINT('Ctrl Pts',(0.760469555880749,1.,1.7918581561088));
#25261=CARTESIAN_POINT('Ctrl Pts',(0.759614401110189,1.,1.78596964884604));
#25262=CARTESIAN_POINT('Ctrl Pts',(0.758650626677518,1.,1.77999411220945));
#25263=CARTESIAN_POINT('Ctrl Pts',(0.757578264077028,1.,1.77394167108292));
#25264=CARTESIAN_POINT('Ctrl Pts',(0.75642189602781,1.,1.76789396002998));
#25265=CARTESIAN_POINT('Ctrl Pts',(0.755220979974461,1.,1.76197817240128));
#25266=CARTESIAN_POINT('Ctrl Pts',(0.754009254027828,1.,1.75631083600019));
#25267=CARTESIAN_POINT('Ctrl Pts',(0.752797683531314,1.,1.75095139468794));
#25268=CARTESIAN_POINT('Ctrl Pts',(0.751555614164482,1.,1.74585086852502));
#25269=CARTESIAN_POINT('Ctrl Pts',(0.750193435981249,1.,1.74080458267114));
#25270=CARTESIAN_POINT('Ctrl Pts',(0.74858246295687,1.,1.7355035168033));
#25271=CARTESIAN_POINT('Ctrl Pts',(0.746574710097752,1.,1.72958533647714));
#25272=CARTESIAN_POINT('Ctrl Pts',(0.744021445433093,1.,1.72268229916769));
#25273=CARTESIAN_POINT('Ctrl Pts',(0.74079516202821,1.,1.71447789751001));
#25274=CARTESIAN_POINT('Ctrl Pts',(0.736799665716932,1.,1.70473309004249));
#25275=CARTESIAN_POINT('Ctrl Pts',(0.731963238685357,1.,1.69326921972915));
#25276=CARTESIAN_POINT('Ctrl Pts',(0.726235967982445,1.,1.67996158451922));
#25277=CARTESIAN_POINT('Ctrl Pts',(0.719585433787949,1.,1.66472880551777));
#25278=CARTESIAN_POINT('Ctrl Pts',(0.711993139340447,1.,1.64752408828442));
#25279=CARTESIAN_POINT('Ctrl Pts',(0.705159151977294,1.,1.6321654166204));
#25280=CARTESIAN_POINT('Ctrl Pts',(0.699605146398836,1.,1.61974673471117));
#25281=CARTESIAN_POINT('Ctrl Pts',(0.69571209787897,1.,1.61106790957619));
#25282=CARTESIAN_POINT('Ctrl Pts',(0.693717979106305,1.,1.60662857109684));
#25283=CARTESIAN_POINT('',(0.7455743247944,0.,2.0698113262342));
#25284=CARTESIAN_POINT('Origin',(0.61342227326009,0.,2.11275013067528));
#25285=CARTESIAN_POINT('',(0.61342227326009,1.,2.11275013067528));
#25286=CARTESIAN_POINT('',(0.7455743247944,1.,2.0698113262342));
#25287=CARTESIAN_POINT('',(0.61342227326009,0.,2.11275013067528));
#25288=CARTESIAN_POINT('Ctrl Pts',(0.383122945602004,-1.,1.7075470150345));
#25289=CARTESIAN_POINT('Ctrl Pts',(0.383122945602004,1.,1.7075470150345));
#25290=CARTESIAN_POINT('Ctrl Pts',(0.384119047315541,-1.,1.71231062891958));
#25291=CARTESIAN_POINT('Ctrl Pts',(0.384119047315541,1.,1.71231062891958));
#25292=CARTESIAN_POINT('Ctrl Pts',(0.38607079032701,-1.,1.72162022246158));
#25293=CARTESIAN_POINT('Ctrl Pts',(0.38607079032701,1.,1.72162022246158));
#25294=CARTESIAN_POINT('Ctrl Pts',(0.388877023509191,-1.,1.7349317097561));
#25295=CARTESIAN_POINT('Ctrl Pts',(0.388877023509191,1.,1.7349317097561));
#25296=CARTESIAN_POINT('Ctrl Pts',(0.392375812294307,-1.,1.75137405313962));
#25297=CARTESIAN_POINT('Ctrl Pts',(0.392375812294307,1.,1.75137405313962));
#25298=CARTESIAN_POINT('Ctrl Pts',(0.39634619612042,-1.,1.7697556004756));
#25299=CARTESIAN_POINT('Ctrl Pts',(0.39634619612042,1.,1.7697556004756));
#25300=CARTESIAN_POINT('Ctrl Pts',(0.39991940378308,-1.,1.78598826347533));
#25301=CARTESIAN_POINT('Ctrl Pts',(0.39991940378308,1.,1.78598826347533));
#25302=CARTESIAN_POINT('Ctrl Pts',(0.403107976170441,-1.,1.80012077176221));
#25303=CARTESIAN_POINT('Ctrl Pts',(0.403107976170441,1.,1.80012077176221));
#25304=CARTESIAN_POINT('Ctrl Pts',(0.405933518411838,-1.,1.81223801813988));
#25305=CARTESIAN_POINT('Ctrl Pts',(0.405933518411838,1.,1.81223801813988));
#25306=CARTESIAN_POINT('Ctrl Pts',(0.408428948108533,-1.,1.8224702267854));
#25307=CARTESIAN_POINT('Ctrl Pts',(0.408428948108533,1.,1.8224702267854));
#25308=CARTESIAN_POINT('Ctrl Pts',(0.410641256301674,-1.,1.83100408895216));
#25309=CARTESIAN_POINT('Ctrl Pts',(0.410641256301674,1.,1.83100408895216));
#25310=CARTESIAN_POINT('Ctrl Pts',(0.412633125322161,-1.,1.83808953475839));
#25311=CARTESIAN_POINT('Ctrl Pts',(0.412633125322161,1.,1.83808953475839));
#25312=CARTESIAN_POINT('Ctrl Pts',(0.41448743825434,-1.,1.8440575707371));
#25313=CARTESIAN_POINT('Ctrl Pts',(0.41448743825434,1.,1.8440575707371));
#25314=CARTESIAN_POINT('Ctrl Pts',(0.416300022038864,-1.,1.84929312929882));
#25315=CARTESIAN_POINT('Ctrl Pts',(0.416300022038864,1.,1.84929312929882));
#25316=CARTESIAN_POINT('Ctrl Pts',(0.418164129143534,-1.,1.85417632856234));
#25317=CARTESIAN_POINT('Ctrl Pts',(0.418164129143534,1.,1.85417632856234));
#25318=CARTESIAN_POINT('Ctrl Pts',(0.420157287975619,-1.,1.85903281096686));
#25319=CARTESIAN_POINT('Ctrl Pts',(0.420157287975619,1.,1.85903281096686));
#25320=CARTESIAN_POINT('Ctrl Pts',(0.422327307418275,-1.,1.86408083334028));
#25321=CARTESIAN_POINT('Ctrl Pts',(0.422327307418275,1.,1.86408083334028));
#25322=CARTESIAN_POINT('Ctrl Pts',(0.424678177291358,-1.,1.86937803944323));
#25323=CARTESIAN_POINT('Ctrl Pts',(0.424678177291358,1.,1.86937803944323));
#25324=CARTESIAN_POINT('Ctrl Pts',(0.427183828519102,-1.,1.87486989291484));
#25325=CARTESIAN_POINT('Ctrl Pts',(0.427183828519102,1.,1.87486989291484));
#25326=CARTESIAN_POINT('Ctrl Pts',(0.429803062482344,-1.,1.88044229001832));
#25327=CARTESIAN_POINT('Ctrl Pts',(0.429803062482344,1.,1.88044229001832));
#25328=CARTESIAN_POINT('Ctrl Pts',(0.432493038548748,-1.,1.88596913666793));
#25329=CARTESIAN_POINT('Ctrl Pts',(0.432493038548748,1.,1.88596913666793));
#25330=CARTESIAN_POINT('Ctrl Pts',(0.435225660963383,-1.,1.89136993975504));
#25331=CARTESIAN_POINT('Ctrl Pts',(0.435225660963383,1.,1.89136993975504));
#25332=CARTESIAN_POINT('Ctrl Pts',(0.437995003948244,-1.,1.89663648956466));
#25333=CARTESIAN_POINT('Ctrl Pts',(0.437995003948244,1.,1.89663648956466));
#25334=CARTESIAN_POINT('Ctrl Pts',(0.440807833704038,-1.,1.90180124389086));
#25335=CARTESIAN_POINT('Ctrl Pts',(0.440807833704038,1.,1.90180124389086));
#25336=CARTESIAN_POINT('Ctrl Pts',(0.44367755684915,-1.,1.90691756144898));
#25337=CARTESIAN_POINT('Ctrl Pts',(0.44367755684915,1.,1.90691756144898));
#25338=CARTESIAN_POINT('Ctrl Pts',(0.446617343485711,-1.,1.9120369998112));
#25339=CARTESIAN_POINT('Ctrl Pts',(0.446617343485711,1.,1.9120369998112));
#25340=CARTESIAN_POINT('Ctrl Pts',(0.449632260106662,-1.,1.91718342555755));
#25341=CARTESIAN_POINT('Ctrl Pts',(0.449632260106662,1.,1.91718342555755));
#25342=CARTESIAN_POINT('Ctrl Pts',(0.452719478359432,-1.,1.92235380648502));
#25343=CARTESIAN_POINT('Ctrl Pts',(0.452719478359432,1.,1.92235380648502));
#25344=CARTESIAN_POINT('Ctrl Pts',(0.45587200517437,-1.,1.92753067150476));
#25345=CARTESIAN_POINT('Ctrl Pts',(0.45587200517437,1.,1.92753067150476));
#25346=CARTESIAN_POINT('Ctrl Pts',(0.459081234547926,-1.,1.93269066517934));
#25347=CARTESIAN_POINT('Ctrl Pts',(0.459081234547926,1.,1.93269066517934));
#25348=CARTESIAN_POINT('Ctrl Pts',(0.462340031009056,-1.,1.93781486640821));
#25349=CARTESIAN_POINT('Ctrl Pts',(0.462340031009056,1.,1.93781486640821));
#25350=CARTESIAN_POINT('Ctrl Pts',(0.46564546202603,-1.,1.9428979419619));
#25351=CARTESIAN_POINT('Ctrl Pts',(0.46564546202603,1.,1.9428979419619));
#25352=CARTESIAN_POINT('Ctrl Pts',(0.468997482913135,-1.,1.94794381136514));
#25353=CARTESIAN_POINT('Ctrl Pts',(0.468997482913135,1.,1.94794381136514));
#25354=CARTESIAN_POINT('Ctrl Pts',(0.472397672264072,-1.,1.95296148278133));
#25355=CARTESIAN_POINT('Ctrl Pts',(0.472397672264072,1.,1.95296148278133));
#25356=CARTESIAN_POINT('Ctrl Pts',(0.475848034683176,-1.,1.95796111148177));
#25357=CARTESIAN_POINT('Ctrl Pts',(0.475848034683176,1.,1.95796111148177));
#25358=CARTESIAN_POINT('Ctrl Pts',(0.479349583074855,-1.,1.96294933055943));
#25359=CARTESIAN_POINT('Ctrl Pts',(0.479349583074855,1.,1.96294933055943));
#25360=CARTESIAN_POINT('Ctrl Pts',(0.48290166212069,-1.,1.96792703422362));
#25361=CARTESIAN_POINT('Ctrl Pts',(0.48290166212069,1.,1.96792703422362));
#25362=CARTESIAN_POINT('Ctrl Pts',(0.486502692907658,-1.,1.97289186263272));
#25363=CARTESIAN_POINT('Ctrl Pts',(0.486502692907658,1.,1.97289186263272));
#25364=CARTESIAN_POINT('Ctrl Pts',(0.490150627860952,-1.,1.97783973019229));
#25365=CARTESIAN_POINT('Ctrl Pts',(0.490150627860952,1.,1.97783973019229));
#25366=CARTESIAN_POINT('Ctrl Pts',(0.493843476541494,-1.,1.98276658761821));
#25367=CARTESIAN_POINT('Ctrl Pts',(0.493843476541494,1.,1.98276658761821));
#25368=CARTESIAN_POINT('Ctrl Pts',(0.497579909545574,-1.,1.98767044752932));
#25369=CARTESIAN_POINT('Ctrl Pts',(0.497579909545574,1.,1.98767044752932));
#25370=CARTESIAN_POINT('Ctrl Pts',(0.501359287727146,-1.,1.99255149126155));
#25371=CARTESIAN_POINT('Ctrl Pts',(0.501359287727146,1.,1.99255149126155));
#25372=CARTESIAN_POINT('Ctrl Pts',(0.505181361323026,-1.,1.99741107463572));
#25373=CARTESIAN_POINT('Ctrl Pts',(0.505181361323026,1.,1.99741107463572));
#25374=CARTESIAN_POINT('Ctrl Pts',(0.509046069886157,-1.,2.00225107134734));
#25375=CARTESIAN_POINT('Ctrl Pts',(0.509046069886157,1.,2.00225107134734));
#25376=CARTESIAN_POINT('Ctrl Pts',(0.512953306961792,-1.,2.00707309946949));
#25377=CARTESIAN_POINT('Ctrl Pts',(0.512953306961792,1.,2.00707309946949));
#25378=CARTESIAN_POINT('Ctrl Pts',(0.516902681728687,-1.,2.01187773939242));
#25379=CARTESIAN_POINT('Ctrl Pts',(0.516902681728687,1.,2.01187773939242));
#25380=CARTESIAN_POINT('Ctrl Pts',(0.52089359039937,-1.,2.01666477917286));
#25381=CARTESIAN_POINT('Ctrl Pts',(0.52089359039937,1.,2.01666477917286));
#25382=CARTESIAN_POINT('Ctrl Pts',(0.524925318333476,-1.,2.02143356304698));
#25383=CARTESIAN_POINT('Ctrl Pts',(0.524925318333476,1.,2.02143356304698));
#25384=CARTESIAN_POINT('Ctrl Pts',(0.528997127241914,-1.,2.0261832908329));
#25385=CARTESIAN_POINT('Ctrl Pts',(0.528997127241914,1.,2.0261832908329));
#25386=CARTESIAN_POINT('Ctrl Pts',(0.533108355132976,-1.,2.03091336214426));
#25387=CARTESIAN_POINT('Ctrl Pts',(0.533108355132976,1.,2.03091336214426));
#25388=CARTESIAN_POINT('Ctrl Pts',(0.537258489833262,-1.,2.03562362954037));
#25389=CARTESIAN_POINT('Ctrl Pts',(0.537258489833262,1.,2.03562362954037));
#25390=CARTESIAN_POINT('Ctrl Pts',(0.541447120615659,-1.,2.04031422690527));
#25391=CARTESIAN_POINT('Ctrl Pts',(0.541447120615659,1.,2.04031422690527));
#25392=CARTESIAN_POINT('Ctrl Pts',(0.54567390381743,-1.,2.04498544714588));
#25393=CARTESIAN_POINT('Ctrl Pts',(0.54567390381743,1.,2.04498544714588));
#25394=CARTESIAN_POINT('Ctrl Pts',(0.549938525150295,-1.,2.04963761077958));
#25395=CARTESIAN_POINT('Ctrl Pts',(0.549938525150295,1.,2.04963761077958));
#25396=CARTESIAN_POINT('Ctrl Pts',(0.554240657463906,-1.,2.05427091604413));
#25397=CARTESIAN_POINT('Ctrl Pts',(0.554240657463906,1.,2.05427091604413));
#25398=CARTESIAN_POINT('Ctrl Pts',(0.558579940185151,-1.,2.05888537756462));
#25399=CARTESIAN_POINT('Ctrl Pts',(0.558579940185151,1.,2.05888537756462));
#25400=CARTESIAN_POINT('Ctrl Pts',(0.562955993082261,-1.,2.06348090160589));
#25401=CARTESIAN_POINT('Ctrl Pts',(0.562955993082261,1.,2.06348090160589));
#25402=CARTESIAN_POINT('Ctrl Pts',(0.567368421181087,-1.,2.06805732997334));
#25403=CARTESIAN_POINT('Ctrl Pts',(0.567368421181087,1.,2.06805732997334));
#25404=CARTESIAN_POINT('Ctrl Pts',(0.571816823242602,-1.,2.07261449292824));
#25405=CARTESIAN_POINT('Ctrl Pts',(0.571816823242602,1.,2.07261449292824));
#25406=CARTESIAN_POINT('Ctrl Pts',(0.576300797416844,-1.,2.07715226767559));
#25407=CARTESIAN_POINT('Ctrl Pts',(0.576300797416844,1.,2.07715226767559));
#25408=CARTESIAN_POINT('Ctrl Pts',(0.580819952108063,-1.,2.08167059018418));
#25409=CARTESIAN_POINT('Ctrl Pts',(0.580819952108063,1.,2.08167059018418));
#25410=CARTESIAN_POINT('Ctrl Pts',(0.585373918991617,-1.,2.08616943727951));
#25411=CARTESIAN_POINT('Ctrl Pts',(0.585373918991617,1.,2.08616943727951));
#25412=CARTESIAN_POINT('Ctrl Pts',(0.589962365403406,-1.,2.09064881812129));
#25413=CARTESIAN_POINT('Ctrl Pts',(0.589962365403406,1.,2.09064881812129));
#25414=CARTESIAN_POINT('Ctrl Pts',(0.594585006052162,-1.,2.0951087622027));
#25415=CARTESIAN_POINT('Ctrl Pts',(0.594585006052162,1.,2.0951087622027));
#25416=CARTESIAN_POINT('Ctrl Pts',(0.599241616420533,-1.,2.0995493086477));
#25417=CARTESIAN_POINT('Ctrl Pts',(0.599241616420533,1.,2.0995493086477));
#25418=CARTESIAN_POINT('Ctrl Pts',(0.60393203073603,-1.,2.10397049886949));
#25419=CARTESIAN_POINT('Ctrl Pts',(0.60393203073603,1.,2.10397049886949));
#25420=CARTESIAN_POINT('Ctrl Pts',(0.607711315454876,-1.,2.1074919961518));
#25421=CARTESIAN_POINT('Ctrl Pts',(0.607711315454876,1.,2.1074919961518));
#25422=CARTESIAN_POINT('Ctrl Pts',(0.610560911689898,-1.,2.11012443807238));
#25423=CARTESIAN_POINT('Ctrl Pts',(0.610560911689898,1.,2.11012443807238));
#25424=CARTESIAN_POINT('Ctrl Pts',(0.6124673655618,-1.,2.11187554259986));
#25425=CARTESIAN_POINT('Ctrl Pts',(0.6124673655618,1.,2.11187554259986));
#25426=CARTESIAN_POINT('Ctrl Pts',(0.61342227326009,-1.,2.11275013067528));
#25427=CARTESIAN_POINT('Ctrl Pts',(0.61342227326009,1.,2.11275013067528));
#25428=CARTESIAN_POINT('',(0.383122945602004,1.,1.7075470150345));
#25429=CARTESIAN_POINT('Ctrl Pts',(0.383122945602004,1.,1.7075470150345));
#25430=CARTESIAN_POINT('Ctrl Pts',(0.384119047315541,1.,1.71231062891958));
#25431=CARTESIAN_POINT('Ctrl Pts',(0.38607079032701,1.,1.72162022246158));
#25432=CARTESIAN_POINT('Ctrl Pts',(0.388877023509191,1.,1.7349317097561));
#25433=CARTESIAN_POINT('Ctrl Pts',(0.392375812294307,1.,1.75137405313962));
#25434=CARTESIAN_POINT('Ctrl Pts',(0.39634619612042,1.,1.7697556004756));
#25435=CARTESIAN_POINT('Ctrl Pts',(0.39991940378308,1.,1.78598826347533));
#25436=CARTESIAN_POINT('Ctrl Pts',(0.403107976170441,1.,1.80012077176221));
#25437=CARTESIAN_POINT('Ctrl Pts',(0.405933518411838,1.,1.81223801813988));
#25438=CARTESIAN_POINT('Ctrl Pts',(0.408428948108533,1.,1.8224702267854));
#25439=CARTESIAN_POINT('Ctrl Pts',(0.410641256301674,1.,1.83100408895216));
#25440=CARTESIAN_POINT('Ctrl Pts',(0.412633125322161,1.,1.83808953475839));
#25441=CARTESIAN_POINT('Ctrl Pts',(0.41448743825434,1.,1.8440575707371));
#25442=CARTESIAN_POINT('Ctrl Pts',(0.416300022038864,1.,1.84929312929882));
#25443=CARTESIAN_POINT('Ctrl Pts',(0.418164129143534,1.,1.85417632856234));
#25444=CARTESIAN_POINT('Ctrl Pts',(0.420157287975619,1.,1.85903281096686));
#25445=CARTESIAN_POINT('Ctrl Pts',(0.422327307418275,1.,1.86408083334028));
#25446=CARTESIAN_POINT('Ctrl Pts',(0.424678177291358,1.,1.86937803944323));
#25447=CARTESIAN_POINT('Ctrl Pts',(0.427183828519102,1.,1.87486989291484));
#25448=CARTESIAN_POINT('Ctrl Pts',(0.429803062482344,1.,1.88044229001832));
#25449=CARTESIAN_POINT('Ctrl Pts',(0.432493038548748,1.,1.88596913666793));
#25450=CARTESIAN_POINT('Ctrl Pts',(0.435225660963383,1.,1.89136993975504));
#25451=CARTESIAN_POINT('Ctrl Pts',(0.437995003948244,1.,1.89663648956466));
#25452=CARTESIAN_POINT('Ctrl Pts',(0.440807833704038,1.,1.90180124389086));
#25453=CARTESIAN_POINT('Ctrl Pts',(0.44367755684915,1.,1.90691756144898));
#25454=CARTESIAN_POINT('Ctrl Pts',(0.446617343485711,1.,1.9120369998112));
#25455=CARTESIAN_POINT('Ctrl Pts',(0.449632260106662,1.,1.91718342555755));
#25456=CARTESIAN_POINT('Ctrl Pts',(0.452719478359432,1.,1.92235380648502));
#25457=CARTESIAN_POINT('Ctrl Pts',(0.45587200517437,1.,1.92753067150476));
#25458=CARTESIAN_POINT('Ctrl Pts',(0.459081234547926,1.,1.93269066517934));
#25459=CARTESIAN_POINT('Ctrl Pts',(0.462340031009056,1.,1.93781486640821));
#25460=CARTESIAN_POINT('Ctrl Pts',(0.46564546202603,1.,1.9428979419619));
#25461=CARTESIAN_POINT('Ctrl Pts',(0.468997482913135,1.,1.94794381136514));
#25462=CARTESIAN_POINT('Ctrl Pts',(0.472397672264072,1.,1.95296148278133));
#25463=CARTESIAN_POINT('Ctrl Pts',(0.475848034683176,1.,1.95796111148177));
#25464=CARTESIAN_POINT('Ctrl Pts',(0.479349583074855,1.,1.96294933055943));
#25465=CARTESIAN_POINT('Ctrl Pts',(0.48290166212069,1.,1.96792703422362));
#25466=CARTESIAN_POINT('Ctrl Pts',(0.486502692907658,1.,1.97289186263272));
#25467=CARTESIAN_POINT('Ctrl Pts',(0.490150627860952,1.,1.97783973019229));
#25468=CARTESIAN_POINT('Ctrl Pts',(0.493843476541494,1.,1.98276658761821));
#25469=CARTESIAN_POINT('Ctrl Pts',(0.497579909545574,1.,1.98767044752932));
#25470=CARTESIAN_POINT('Ctrl Pts',(0.501359287727146,1.,1.99255149126155));
#25471=CARTESIAN_POINT('Ctrl Pts',(0.505181361323026,1.,1.99741107463572));
#25472=CARTESIAN_POINT('Ctrl Pts',(0.509046069886157,1.,2.00225107134734));
#25473=CARTESIAN_POINT('Ctrl Pts',(0.512953306961792,1.,2.00707309946949));
#25474=CARTESIAN_POINT('Ctrl Pts',(0.516902681728687,1.,2.01187773939242));
#25475=CARTESIAN_POINT('Ctrl Pts',(0.52089359039937,1.,2.01666477917286));
#25476=CARTESIAN_POINT('Ctrl Pts',(0.524925318333476,1.,2.02143356304698));
#25477=CARTESIAN_POINT('Ctrl Pts',(0.528997127241914,1.,2.0261832908329));
#25478=CARTESIAN_POINT('Ctrl Pts',(0.533108355132976,1.,2.03091336214426));
#25479=CARTESIAN_POINT('Ctrl Pts',(0.537258489833262,1.,2.03562362954037));
#25480=CARTESIAN_POINT('Ctrl Pts',(0.541447120615659,1.,2.04031422690527));
#25481=CARTESIAN_POINT('Ctrl Pts',(0.54567390381743,1.,2.04498544714588));
#25482=CARTESIAN_POINT('Ctrl Pts',(0.549938525150295,1.,2.04963761077958));
#25483=CARTESIAN_POINT('Ctrl Pts',(0.554240657463906,1.,2.05427091604413));
#25484=CARTESIAN_POINT('Ctrl Pts',(0.558579940185151,1.,2.05888537756462));
#25485=CARTESIAN_POINT('Ctrl Pts',(0.562955993082261,1.,2.06348090160589));
#25486=CARTESIAN_POINT('Ctrl Pts',(0.567368421181087,1.,2.06805732997334));
#25487=CARTESIAN_POINT('Ctrl Pts',(0.571816823242602,1.,2.07261449292824));
#25488=CARTESIAN_POINT('Ctrl Pts',(0.576300797416844,1.,2.07715226767559));
#25489=CARTESIAN_POINT('Ctrl Pts',(0.580819952108063,1.,2.08167059018418));
#25490=CARTESIAN_POINT('Ctrl Pts',(0.585373918991617,1.,2.08616943727951));
#25491=CARTESIAN_POINT('Ctrl Pts',(0.589962365403406,1.,2.09064881812129));
#25492=CARTESIAN_POINT('Ctrl Pts',(0.594585006052162,1.,2.0951087622027));
#25493=CARTESIAN_POINT('Ctrl Pts',(0.599241616420533,1.,2.0995493086477));
#25494=CARTESIAN_POINT('Ctrl Pts',(0.60393203073603,1.,2.10397049886949));
#25495=CARTESIAN_POINT('Ctrl Pts',(0.607711315454876,1.,2.1074919961518));
#25496=CARTESIAN_POINT('Ctrl Pts',(0.610560911689898,1.,2.11012443807238));
#25497=CARTESIAN_POINT('Ctrl Pts',(0.6124673655618,1.,2.11187554259986));
#25498=CARTESIAN_POINT('Ctrl Pts',(0.61342227326009,1.,2.11275013067528));
#25499=CARTESIAN_POINT('',(0.383122945602003,0.,1.7075470150345));
#25500=CARTESIAN_POINT('Origin',(0.,0.,0.));
#25501=CARTESIAN_POINT('',(0.163289472382896,1.,1.74236521665491));
#25502=CARTESIAN_POINT('Origin',(0.,1.,0.));
#25503=CARTESIAN_POINT('',(0.163289472382896,0.,1.74236521665491));
#25504=CARTESIAN_POINT('Ctrl Pts',(0.0694764450219578,-1.,2.19890268624765));
#25505=CARTESIAN_POINT('Ctrl Pts',(0.0694764450219578,1.,2.19890268624765));
#25506=CARTESIAN_POINT('Ctrl Pts',(0.0701143536325487,-1.,2.19777582085423));
#25507=CARTESIAN_POINT('Ctrl Pts',(0.0701143536325487,1.,2.19777582085423));
#25508=CARTESIAN_POINT('Ctrl Pts',(0.0713863779526151,-1.,2.19552129484002));
#25509=CARTESIAN_POINT('Ctrl Pts',(0.0713863779526151,1.,2.19552129484002));
#25510=CARTESIAN_POINT('Ctrl Pts',(0.0732830357306722,-1.,2.19213712013662));
#25511=CARTESIAN_POINT('Ctrl Pts',(0.0732830357306722,1.,2.19213712013662));
#25512=CARTESIAN_POINT('Ctrl Pts',(0.0757891465836145,-1.,2.1876201139953));
#25513=CARTESIAN_POINT('Ctrl Pts',(0.0757891465836145,1.,2.1876201139953));
#25514=CARTESIAN_POINT('Ctrl Pts',(0.078883772768524,-1.,2.18196589448887));
#25515=CARTESIAN_POINT('Ctrl Pts',(0.078883772768524,1.,2.18196589448887));
#25516=CARTESIAN_POINT('Ctrl Pts',(0.0819402680872763,-1.,2.176303712113));
#25517=CARTESIAN_POINT('Ctrl Pts',(0.0819402680872763,1.,2.176303712113));
#25518=CARTESIAN_POINT('Ctrl Pts',(0.084958462083537,-1.,2.17063357870952));
#25519=CARTESIAN_POINT('Ctrl Pts',(0.084958462083537,1.,2.17063357870952));
#25520=CARTESIAN_POINT('Ctrl Pts',(0.087938129138692,-1.,2.16495552645014));
#25521=CARTESIAN_POINT('Ctrl Pts',(0.087938129138692,1.,2.16495552645014));
#25522=CARTESIAN_POINT('Ctrl Pts',(0.0908789888107263,-1.,2.15926961544516));
#25523=CARTESIAN_POINT('Ctrl Pts',(0.0908789888107263,1.,2.15926961544516));
#25524=CARTESIAN_POINT('Ctrl Pts',(0.0937807218867641,-1.,2.1535759397817));
#25525=CARTESIAN_POINT('Ctrl Pts',(0.0937807218867641,1.,2.1535759397817));
#25526=CARTESIAN_POINT('Ctrl Pts',(0.0966429852305456,-1.,2.14787463531795));
#25527=CARTESIAN_POINT('Ctrl Pts',(0.0966429852305456,1.,2.14787463531795));
#25528=CARTESIAN_POINT('Ctrl Pts',(0.0994654261990913,-1.,2.14216588396025));
#25529=CARTESIAN_POINT('Ctrl Pts',(0.0994654261990913,1.,2.14216588396025));
#25530=CARTESIAN_POINT('Ctrl Pts',(0.1022477005561,-1.,2.13644992667165));
#25531=CARTESIAN_POINT('Ctrl Pts',(0.1022477005561,1.,2.13644992667165));
#25532=CARTESIAN_POINT('Ctrl Pts',(0.104989479152739,-1.,2.13072704887293));
#25533=CARTESIAN_POINT('Ctrl Pts',(0.104989479152739,1.,2.13072704887293));
#25534=CARTESIAN_POINT('Ctrl Pts',(0.10769043523109,-1.,2.12499752307));
#25535=CARTESIAN_POINT('Ctrl Pts',(0.10769043523109,1.,2.12499752307));
#25536=CARTESIAN_POINT('Ctrl Pts',(0.110350236135025,-1.,2.11926155590865));
#25537=CARTESIAN_POINT('Ctrl Pts',(0.110350236135025,1.,2.11926155590865));
#25538=CARTESIAN_POINT('Ctrl Pts',(0.112968534419737,-1.,2.11351924490306));
#25539=CARTESIAN_POINT('Ctrl Pts',(0.112968534419737,1.,2.11351924490306));
#25540=CARTESIAN_POINT('Ctrl Pts',(0.115544957687926,-1.,2.10777050261309));
#25541=CARTESIAN_POINT('Ctrl Pts',(0.115544957687926,1.,2.10777050261309));
#25542=CARTESIAN_POINT('Ctrl Pts',(0.118079107988355,-1.,2.102015121329));
#25543=CARTESIAN_POINT('Ctrl Pts',(0.118079107988355,1.,2.102015121329));
#25544=CARTESIAN_POINT('Ctrl Pts',(0.120570567965122,-1.,2.0962529286773));
#25545=CARTESIAN_POINT('Ctrl Pts',(0.120570567965122,1.,2.0962529286773));
#25546=CARTESIAN_POINT('Ctrl Pts',(0.123018905621083,-1.,2.09048392424825));
#25547=CARTESIAN_POINT('Ctrl Pts',(0.123018905621083,1.,2.09048392424825));
#25548=CARTESIAN_POINT('Ctrl Pts',(0.125423679412061,-1.,2.08470840653643));
#25549=CARTESIAN_POINT('Ctrl Pts',(0.125423679412061,1.,2.08470840653643));
#25550=CARTESIAN_POINT('Ctrl Pts',(0.12778444527612,-1.,2.07892715110987));
#25551=CARTESIAN_POINT('Ctrl Pts',(0.12778444527612,1.,2.07892715110987));
#25552=CARTESIAN_POINT('Ctrl Pts',(0.130100748328403,-1.,2.07314114713063));
#25553=CARTESIAN_POINT('Ctrl Pts',(0.130100748328403,1.,2.07314114713063));
#25554=CARTESIAN_POINT('Ctrl Pts',(0.13237211154771,-1.,2.06735123910326));
#25555=CARTESIAN_POINT('Ctrl Pts',(0.13237211154771,1.,2.06735123910326));
#25556=CARTESIAN_POINT('Ctrl Pts',(0.134598026192106,-1.,2.06155781517842));
#25557=CARTESIAN_POINT('Ctrl Pts',(0.134598026192106,1.,2.06155781517842));
#25558=CARTESIAN_POINT('Ctrl Pts',(0.136777941218043,-1.,2.05576044414264));
#25559=CARTESIAN_POINT('Ctrl Pts',(0.136777941218043,1.,2.05576044414264));
#25560=CARTESIAN_POINT('Ctrl Pts',(0.138911255368966,-1.,2.04995762001328));
#25561=CARTESIAN_POINT('Ctrl Pts',(0.138911255368966,1.,2.04995762001328));
#25562=CARTESIAN_POINT('Ctrl Pts',(0.140997332152546,-1.,2.04414757947916));
#25563=CARTESIAN_POINT('Ctrl Pts',(0.140997332152546,1.,2.04414757947916));
#25564=CARTESIAN_POINT('Ctrl Pts',(0.143035515058208,-1.,2.03832911025912));
#25565=CARTESIAN_POINT('Ctrl Pts',(0.143035515058208,1.,2.03832911025912));
#25566=CARTESIAN_POINT('Ctrl Pts',(0.145025140186057,-1.,2.03250223739942));
#25567=CARTESIAN_POINT('Ctrl Pts',(0.145025140186057,1.,2.03250223739942));
#25568=CARTESIAN_POINT('Ctrl Pts',(0.146965557332583,-1.,2.02666926182017));
#25569=CARTESIAN_POINT('Ctrl Pts',(0.146965557332583,1.,2.02666926182017));
#25570=CARTESIAN_POINT('Ctrl Pts',(0.148856124775337,-1.,2.02083464969894));
#25571=CARTESIAN_POINT('Ctrl Pts',(0.148856124775337,1.,2.02083464969894));
#25572=CARTESIAN_POINT('Ctrl Pts',(0.150696157673078,-1.,2.01500291940238));
#25573=CARTESIAN_POINT('Ctrl Pts',(0.150696157673078,1.,2.01500291940238));
#25574=CARTESIAN_POINT('Ctrl Pts',(0.152484883621449,-1.,2.00917680318424));
#25575=CARTESIAN_POINT('Ctrl Pts',(0.152484883621449,1.,2.00917680318424));
#25576=CARTESIAN_POINT('Ctrl Pts',(0.154221403049722,-1.,2.00335565310543));
#25577=CARTESIAN_POINT('Ctrl Pts',(0.154221403049722,1.,2.00335565310543));
#25578=CARTESIAN_POINT('Ctrl Pts',(0.155904629548783,-1.,1.99753284771497));
#25579=CARTESIAN_POINT('Ctrl Pts',(0.155904629548783,1.,1.99753284771497));
#25580=CARTESIAN_POINT('Ctrl Pts',(0.157533331459227,-1.,1.99169810931908));
#25581=CARTESIAN_POINT('Ctrl Pts',(0.157533331459227,1.,1.99169810931908));
#25582=CARTESIAN_POINT('Ctrl Pts',(0.159106226437299,-1.,1.98584238283292));
#25583=CARTESIAN_POINT('Ctrl Pts',(0.159106226437299,1.,1.98584238283292));
#25584=CARTESIAN_POINT('Ctrl Pts',(0.160622060784611,-1.,1.97996195437559));
#25585=CARTESIAN_POINT('Ctrl Pts',(0.160622060784611,1.,1.97996195437559));
#25586=CARTESIAN_POINT('Ctrl Pts',(0.162079693556288,-1.,1.97406280235188));
#25587=CARTESIAN_POINT('Ctrl Pts',(0.162079693556288,1.,1.97406280235188));
#25588=CARTESIAN_POINT('Ctrl Pts',(0.163478185457734,-1.,1.96816512677967));
#25589=CARTESIAN_POINT('Ctrl Pts',(0.163478185457734,1.,1.96816512677967));
#25590=CARTESIAN_POINT('Ctrl Pts',(0.164816568920269,-1.,1.96229379940136));
#25591=CARTESIAN_POINT('Ctrl Pts',(0.164816568920269,1.,1.96229379940136));
#25592=CARTESIAN_POINT('Ctrl Pts',(0.166093592002812,-1.,1.9564675971873));
#25593=CARTESIAN_POINT('Ctrl Pts',(0.166093592002812,1.,1.9564675971873));
#25594=CARTESIAN_POINT('Ctrl Pts',(0.167307501784475,-1.,1.95069027794294));
#25595=CARTESIAN_POINT('Ctrl Pts',(0.167307501784475,1.,1.95069027794294));
#25596=CARTESIAN_POINT('Ctrl Pts',(0.168455741607556,-1.,1.94493757756931));
#25597=CARTESIAN_POINT('Ctrl Pts',(0.168455741607556,1.,1.94493757756931));
#25598=CARTESIAN_POINT('Ctrl Pts',(0.16953490481749,-1.,1.93915639211581));
#25599=CARTESIAN_POINT('Ctrl Pts',(0.16953490481749,1.,1.93915639211581));
#25600=CARTESIAN_POINT('Ctrl Pts',(0.170541253116201,-1.,1.93329183155539));
#25601=CARTESIAN_POINT('Ctrl Pts',(0.170541253116201,1.,1.93329183155539));
#25602=CARTESIAN_POINT('Ctrl Pts',(0.171471191532988,-1.,1.92731093582036));
#25603=CARTESIAN_POINT('Ctrl Pts',(0.171471191532988,1.,1.92731093582036));
#25604=CARTESIAN_POINT('Ctrl Pts',(0.172321621259513,-1.,1.9212233439798));
#25605=CARTESIAN_POINT('Ctrl Pts',(0.172321621259513,1.,1.9212233439798));
#25606=CARTESIAN_POINT('Ctrl Pts',(0.173090695383496,-1.,1.91511429159527));
#25607=CARTESIAN_POINT('Ctrl Pts',(0.173090695383496,1.,1.91511429159527));
#25608=CARTESIAN_POINT('Ctrl Pts',(0.173776635257816,-1.,1.90911693975267));
#25609=CARTESIAN_POINT('Ctrl Pts',(0.173776635257816,1.,1.90911693975267));
#25610=CARTESIAN_POINT('Ctrl Pts',(0.174375518661085,-1.,1.90335253862834));
#25611=CARTESIAN_POINT('Ctrl Pts',(0.174375518661085,1.,1.90335253862834));
#25612=CARTESIAN_POINT('Ctrl Pts',(0.174879405091263,-1.,1.89788101117132));
#25613=CARTESIAN_POINT('Ctrl Pts',(0.174879405091263,1.,1.89788101117132));
#25614=CARTESIAN_POINT('Ctrl Pts',(0.175274276190844,-1.,1.892646301985));
#25615=CARTESIAN_POINT('Ctrl Pts',(0.175274276190844,1.,1.892646301985));
#25616=CARTESIAN_POINT('Ctrl Pts',(0.175538155840648,-1.,1.88742606273259));
#25617=CARTESIAN_POINT('Ctrl Pts',(0.175538155840648,1.,1.88742606273259));
#25618=CARTESIAN_POINT('Ctrl Pts',(0.175644148889698,-1.,1.88188663145367));
#25619=CARTESIAN_POINT('Ctrl Pts',(0.175644148889698,1.,1.88188663145367));
#25620=CARTESIAN_POINT('Ctrl Pts',(0.175563480746485,-1.,1.87563767773588));
#25621=CARTESIAN_POINT('Ctrl Pts',(0.175563480746485,1.,1.87563767773588));
#25622=CARTESIAN_POINT('Ctrl Pts',(0.175268337590757,-1.,1.86828349694799));
#25623=CARTESIAN_POINT('Ctrl Pts',(0.175268337590757,1.,1.86828349694799));
#25624=CARTESIAN_POINT('Ctrl Pts',(0.17473525927603,-1.,1.85948367088837));
#25625=CARTESIAN_POINT('Ctrl Pts',(0.17473525927603,1.,1.85948367088837));
#25626=CARTESIAN_POINT('Ctrl Pts',(0.173946627587731,-1.,1.8489811319852));
#25627=CARTESIAN_POINT('Ctrl Pts',(0.173946627587731,1.,1.8489811319852));
#25628=CARTESIAN_POINT('Ctrl Pts',(0.1728894428919,-1.,1.83658380527692));
#25629=CARTESIAN_POINT('Ctrl Pts',(0.1728894428919,1.,1.83658380527692));
#25630=CARTESIAN_POINT('Ctrl Pts',(0.171554770204119,-1.,1.82215766811545));
#25631=CARTESIAN_POINT('Ctrl Pts',(0.171554770204119,1.,1.82215766811545));
#25632=CARTESIAN_POINT('Ctrl Pts',(0.169936923904608,-1.,1.80561530629706));
#25633=CARTESIAN_POINT('Ctrl Pts',(0.169936923904608,1.,1.80561530629706));
#25634=CARTESIAN_POINT('Ctrl Pts',(0.168032772805197,-1.,1.7869064998507));
#25635=CARTESIAN_POINT('Ctrl Pts',(0.168032772805197,1.,1.7869064998507));
#25636=CARTESIAN_POINT('Ctrl Pts',(0.1662793551464,-1.,1.77018771684844));
#25637=CARTESIAN_POINT('Ctrl Pts',(0.1662793551464,1.,1.77018771684844));
#25638=CARTESIAN_POINT('Ctrl Pts',(0.164834765707158,-1.,1.75666056638427));
#25639=CARTESIAN_POINT('Ctrl Pts',(0.164834765707158,1.,1.75666056638427));
#25640=CARTESIAN_POINT('Ctrl Pts',(0.163814161002002,-1.,1.7472034950333));
#25641=CARTESIAN_POINT('Ctrl Pts',(0.163814161002002,1.,1.7472034950333));
#25642=CARTESIAN_POINT('Ctrl Pts',(0.163289472382896,-1.,1.74236521665491));
#25643=CARTESIAN_POINT('Ctrl Pts',(0.163289472382896,1.,1.74236521665491));
#25644=CARTESIAN_POINT('',(0.0694764450219578,1.,2.19890268624765));
#25645=CARTESIAN_POINT('Ctrl Pts',(0.0694764450219578,1.,2.19890268624765));
#25646=CARTESIAN_POINT('Ctrl Pts',(0.0701143536325487,1.,2.19777582085423));
#25647=CARTESIAN_POINT('Ctrl Pts',(0.0713863779526151,1.,2.19552129484002));
#25648=CARTESIAN_POINT('Ctrl Pts',(0.0732830357306722,1.,2.19213712013662));
#25649=CARTESIAN_POINT('Ctrl Pts',(0.0757891465836145,1.,2.1876201139953));
#25650=CARTESIAN_POINT('Ctrl Pts',(0.078883772768524,1.,2.18196589448887));
#25651=CARTESIAN_POINT('Ctrl Pts',(0.0819402680872763,1.,2.176303712113));
#25652=CARTESIAN_POINT('Ctrl Pts',(0.084958462083537,1.,2.17063357870952));
#25653=CARTESIAN_POINT('Ctrl Pts',(0.087938129138692,1.,2.16495552645014));
#25654=CARTESIAN_POINT('Ctrl Pts',(0.0908789888107263,1.,2.15926961544516));
#25655=CARTESIAN_POINT('Ctrl Pts',(0.0937807218867641,1.,2.1535759397817));
#25656=CARTESIAN_POINT('Ctrl Pts',(0.0966429852305456,1.,2.14787463531795));
#25657=CARTESIAN_POINT('Ctrl Pts',(0.0994654261990913,1.,2.14216588396025));
#25658=CARTESIAN_POINT('Ctrl Pts',(0.1022477005561,1.,2.13644992667165));
#25659=CARTESIAN_POINT('Ctrl Pts',(0.104989479152739,1.,2.13072704887293));
#25660=CARTESIAN_POINT('Ctrl Pts',(0.10769043523109,1.,2.12499752307));
#25661=CARTESIAN_POINT('Ctrl Pts',(0.110350236135025,1.,2.11926155590865));
#25662=CARTESIAN_POINT('Ctrl Pts',(0.112968534419737,1.,2.11351924490306));
#25663=CARTESIAN_POINT('Ctrl Pts',(0.115544957687926,1.,2.10777050261309));
#25664=CARTESIAN_POINT('Ctrl Pts',(0.118079107988355,1.,2.102015121329));
#25665=CARTESIAN_POINT('Ctrl Pts',(0.120570567965122,1.,2.0962529286773));
#25666=CARTESIAN_POINT('Ctrl Pts',(0.123018905621083,1.,2.09048392424825));
#25667=CARTESIAN_POINT('Ctrl Pts',(0.125423679412061,1.,2.08470840653643));
#25668=CARTESIAN_POINT('Ctrl Pts',(0.12778444527612,1.,2.07892715110987));
#25669=CARTESIAN_POINT('Ctrl Pts',(0.130100748328403,1.,2.07314114713063));
#25670=CARTESIAN_POINT('Ctrl Pts',(0.13237211154771,1.,2.06735123910326));
#25671=CARTESIAN_POINT('Ctrl Pts',(0.134598026192106,1.,2.06155781517842));
#25672=CARTESIAN_POINT('Ctrl Pts',(0.136777941218043,1.,2.05576044414264));
#25673=CARTESIAN_POINT('Ctrl Pts',(0.138911255368966,1.,2.04995762001328));
#25674=CARTESIAN_POINT('Ctrl Pts',(0.140997332152546,1.,2.04414757947916));
#25675=CARTESIAN_POINT('Ctrl Pts',(0.143035515058208,1.,2.03832911025912));
#25676=CARTESIAN_POINT('Ctrl Pts',(0.145025140186057,1.,2.03250223739942));
#25677=CARTESIAN_POINT('Ctrl Pts',(0.146965557332583,1.,2.02666926182017));
#25678=CARTESIAN_POINT('Ctrl Pts',(0.148856124775337,1.,2.02083464969894));
#25679=CARTESIAN_POINT('Ctrl Pts',(0.150696157673078,1.,2.01500291940238));
#25680=CARTESIAN_POINT('Ctrl Pts',(0.152484883621449,1.,2.00917680318424));
#25681=CARTESIAN_POINT('Ctrl Pts',(0.154221403049722,1.,2.00335565310543));
#25682=CARTESIAN_POINT('Ctrl Pts',(0.155904629548783,1.,1.99753284771497));
#25683=CARTESIAN_POINT('Ctrl Pts',(0.157533331459227,1.,1.99169810931908));
#25684=CARTESIAN_POINT('Ctrl Pts',(0.159106226437299,1.,1.98584238283292));
#25685=CARTESIAN_POINT('Ctrl Pts',(0.160622060784611,1.,1.97996195437559));
#25686=CARTESIAN_POINT('Ctrl Pts',(0.162079693556288,1.,1.97406280235188));
#25687=CARTESIAN_POINT('Ctrl Pts',(0.163478185457734,1.,1.96816512677967));
#25688=CARTESIAN_POINT('Ctrl Pts',(0.164816568920269,1.,1.96229379940136));
#25689=CARTESIAN_POINT('Ctrl Pts',(0.166093592002812,1.,1.9564675971873));
#25690=CARTESIAN_POINT('Ctrl Pts',(0.167307501784475,1.,1.95069027794294));
#25691=CARTESIAN_POINT('Ctrl Pts',(0.168455741607556,1.,1.94493757756931));
#25692=CARTESIAN_POINT('Ctrl Pts',(0.16953490481749,1.,1.93915639211581));
#25693=CARTESIAN_POINT('Ctrl Pts',(0.170541253116201,1.,1.93329183155539));
#25694=CARTESIAN_POINT('Ctrl Pts',(0.171471191532988,1.,1.92731093582036));
#25695=CARTESIAN_POINT('Ctrl Pts',(0.172321621259513,1.,1.9212233439798));
#25696=CARTESIAN_POINT('Ctrl Pts',(0.173090695383496,1.,1.91511429159527));
#25697=CARTESIAN_POINT('Ctrl Pts',(0.173776635257816,1.,1.90911693975267));
#25698=CARTESIAN_POINT('Ctrl Pts',(0.174375518661085,1.,1.90335253862834));
#25699=CARTESIAN_POINT('Ctrl Pts',(0.174879405091263,1.,1.89788101117132));
#25700=CARTESIAN_POINT('Ctrl Pts',(0.175274276190844,1.,1.892646301985));
#25701=CARTESIAN_POINT('Ctrl Pts',(0.175538155840648,1.,1.88742606273259));
#25702=CARTESIAN_POINT('Ctrl Pts',(0.175644148889698,1.,1.88188663145367));
#25703=CARTESIAN_POINT('Ctrl Pts',(0.175563480746485,1.,1.87563767773588));
#25704=CARTESIAN_POINT('Ctrl Pts',(0.175268337590757,1.,1.86828349694799));
#25705=CARTESIAN_POINT('Ctrl Pts',(0.17473525927603,1.,1.85948367088837));
#25706=CARTESIAN_POINT('Ctrl Pts',(0.173946627587731,1.,1.8489811319852));
#25707=CARTESIAN_POINT('Ctrl Pts',(0.1728894428919,1.,1.83658380527692));
#25708=CARTESIAN_POINT('Ctrl Pts',(0.171554770204119,1.,1.82215766811545));
#25709=CARTESIAN_POINT('Ctrl Pts',(0.169936923904608,1.,1.80561530629706));
#25710=CARTESIAN_POINT('Ctrl Pts',(0.168032772805197,1.,1.7869064998507));
#25711=CARTESIAN_POINT('Ctrl Pts',(0.1662793551464,1.,1.77018771684844));
#25712=CARTESIAN_POINT('Ctrl Pts',(0.164834765707158,1.,1.75666056638427));
#25713=CARTESIAN_POINT('Ctrl Pts',(0.163814161002002,1.,1.7472034950333));
#25714=CARTESIAN_POINT('Ctrl Pts',(0.163289472382896,1.,1.74236521665491));
#25715=CARTESIAN_POINT('',(0.0694764450219578,0.,2.19890268624765));
#25716=CARTESIAN_POINT('Origin',(-0.0694764450219586,0.,2.19890268624765));
#25717=CARTESIAN_POINT('',(-0.0694764450219586,1.,2.19890268624765));
#25718=CARTESIAN_POINT('',(0.0694764450219578,1.,2.19890268624765));
#25719=CARTESIAN_POINT('',(-0.0694764450219586,0.,2.19890268624765));
#25720=CARTESIAN_POINT('Ctrl Pts',(-0.163289472382896,-1.,1.74236521665491));
#25721=CARTESIAN_POINT('Ctrl Pts',(-0.163289472382896,1.,1.74236521665491));
#25722=CARTESIAN_POINT('Ctrl Pts',(-0.163814161002474,-1.,1.74720349503904));
#25723=CARTESIAN_POINT('Ctrl Pts',(-0.163814161002474,1.,1.74720349503904));
#25724=CARTESIAN_POINT('Ctrl Pts',(-0.164834765708484,-1.,1.75666056640041));
#25725=CARTESIAN_POINT('Ctrl Pts',(-0.164834765708484,1.,1.75666056640041));
#25726=CARTESIAN_POINT('Ctrl Pts',(-0.166279355148738,-1.,1.77018771687692));
#25727=CARTESIAN_POINT('Ctrl Pts',(-0.166279355148738,1.,1.77018771687692));
#25728=CARTESIAN_POINT('Ctrl Pts',(-0.16803277280837,-1.,1.78690649988931));
#25729=CARTESIAN_POINT('Ctrl Pts',(-0.16803277280837,1.,1.78690649988931));
#25730=CARTESIAN_POINT('Ctrl Pts',(-0.169936923908078,-1.,1.80561530633924));
#25731=CARTESIAN_POINT('Ctrl Pts',(-0.169936923908078,1.,1.80561530633924));
#25732=CARTESIAN_POINT('Ctrl Pts',(-0.171554770207306,-1.,1.82215766815414));
#25733=CARTESIAN_POINT('Ctrl Pts',(-0.171554770207306,1.,1.82215766815414));
#25734=CARTESIAN_POINT('Ctrl Pts',(-0.17288944289442,-1.,1.83658380530747));
#25735=CARTESIAN_POINT('Ctrl Pts',(-0.17288944289442,1.,1.83658380530747));
#25736=CARTESIAN_POINT('Ctrl Pts',(-0.173946627589401,-1.,1.84898113200543));
#25737=CARTESIAN_POINT('Ctrl Pts',(-0.173946627589401,1.,1.84898113200543));
#25738=CARTESIAN_POINT('Ctrl Pts',(-0.174735259276856,-1.,1.85948367089838));
#25739=CARTESIAN_POINT('Ctrl Pts',(-0.174735259276856,1.,1.85948367089838));
#25740=CARTESIAN_POINT('Ctrl Pts',(-0.175268337590901,-1.,1.86828349694972));
#25741=CARTESIAN_POINT('Ctrl Pts',(-0.175268337590901,1.,1.86828349694972));
#25742=CARTESIAN_POINT('Ctrl Pts',(-0.175563480746206,-1.,1.87563767773249));
#25743=CARTESIAN_POINT('Ctrl Pts',(-0.175563480746206,1.,1.87563767773249));
#25744=CARTESIAN_POINT('Ctrl Pts',(-0.175644148889271,-1.,1.88188663144846));
#25745=CARTESIAN_POINT('Ctrl Pts',(-0.175644148889271,1.,1.88188663144846));
#25746=CARTESIAN_POINT('Ctrl Pts',(-0.175538155840286,-1.,1.88742606272818));
#25747=CARTESIAN_POINT('Ctrl Pts',(-0.175538155840286,1.,1.88742606272818));
#25748=CARTESIAN_POINT('Ctrl Pts',(-0.175274276190664,-1.,1.89264630198279));
#25749=CARTESIAN_POINT('Ctrl Pts',(-0.175274276190664,1.,1.89264630198279));
#25750=CARTESIAN_POINT('Ctrl Pts',(-0.174879405091277,-1.,1.89788101117148));
#25751=CARTESIAN_POINT('Ctrl Pts',(-0.174879405091277,1.,1.89788101117148));
#25752=CARTESIAN_POINT('Ctrl Pts',(-0.174375518661222,-1.,1.90335253863003));
#25753=CARTESIAN_POINT('Ctrl Pts',(-0.174375518661222,1.,1.90335253863003));
#25754=CARTESIAN_POINT('Ctrl Pts',(-0.173776635257984,-1.,1.90911693975475));
#25755=CARTESIAN_POINT('Ctrl Pts',(-0.173776635257984,1.,1.90911693975475));
#25756=CARTESIAN_POINT('Ctrl Pts',(-0.173090695383619,-1.,1.91511429159681));
#25757=CARTESIAN_POINT('Ctrl Pts',(-0.173090695383619,1.,1.91511429159681));
#25758=CARTESIAN_POINT('Ctrl Pts',(-0.172321621259557,-1.,1.92122334398034));
#25759=CARTESIAN_POINT('Ctrl Pts',(-0.172321621259557,1.,1.92122334398034));
#25760=CARTESIAN_POINT('Ctrl Pts',(-0.17147119153296,-1.,1.92731093582));
#25761=CARTESIAN_POINT('Ctrl Pts',(-0.17147119153296,1.,1.92731093582));
#25762=CARTESIAN_POINT('Ctrl Pts',(-0.170541253116136,-1.,1.93329183155455));
#25763=CARTESIAN_POINT('Ctrl Pts',(-0.170541253116136,1.,1.93329183155455));
#25764=CARTESIAN_POINT('Ctrl Pts',(-0.169534904817425,-1.,1.93915639211497));
#25765=CARTESIAN_POINT('Ctrl Pts',(-0.169534904817425,1.,1.93915639211497));
#25766=CARTESIAN_POINT('Ctrl Pts',(-0.168455741607516,-1.,1.94493757756879));
#25767=CARTESIAN_POINT('Ctrl Pts',(-0.168455741607516,1.,1.94493757756879));
#25768=CARTESIAN_POINT('Ctrl Pts',(-0.167307501784469,-1.,1.95069027794286));
#25769=CARTESIAN_POINT('Ctrl Pts',(-0.167307501784469,1.,1.95069027794286));
#25770=CARTESIAN_POINT('Ctrl Pts',(-0.166093592002833,-1.,1.95646759718755));
#25771=CARTESIAN_POINT('Ctrl Pts',(-0.166093592002833,1.,1.95646759718755));
#25772=CARTESIAN_POINT('Ctrl Pts',(-0.1648165689203,-1.,1.96229379940174));
#25773=CARTESIAN_POINT('Ctrl Pts',(-0.1648165689203,1.,1.96229379940174));
#25774=CARTESIAN_POINT('Ctrl Pts',(-0.16347818545776,-1.,1.96816512678));
#25775=CARTESIAN_POINT('Ctrl Pts',(-0.16347818545776,1.,1.96816512678));
#25776=CARTESIAN_POINT('Ctrl Pts',(-0.162079693556302,-1.,1.97406280235204));
#25777=CARTESIAN_POINT('Ctrl Pts',(-0.162079693556302,1.,1.97406280235204));
#25778=CARTESIAN_POINT('Ctrl Pts',(-0.16062206078461,-1.,1.97996195437557));
#25779=CARTESIAN_POINT('Ctrl Pts',(-0.16062206078461,1.,1.97996195437557));
#25780=CARTESIAN_POINT('Ctrl Pts',(-0.159106226437289,-1.,1.98584238283279));
#25781=CARTESIAN_POINT('Ctrl Pts',(-0.159106226437289,1.,1.98584238283279));
#25782=CARTESIAN_POINT('Ctrl Pts',(-0.157533331459215,-1.,1.99169810931893));
#25783=CARTESIAN_POINT('Ctrl Pts',(-0.157533331459215,1.,1.99169810931893));
#25784=CARTESIAN_POINT('Ctrl Pts',(-0.155904629548775,-1.,1.99753284771487));
#25785=CARTESIAN_POINT('Ctrl Pts',(-0.155904629548775,1.,1.99753284771487));
#25786=CARTESIAN_POINT('Ctrl Pts',(-0.154221403049719,-1.,2.00335565310539));
#25787=CARTESIAN_POINT('Ctrl Pts',(-0.154221403049719,1.,2.00335565310539));
#25788=CARTESIAN_POINT('Ctrl Pts',(-0.152484883621452,-1.,2.00917680318426));
#25789=CARTESIAN_POINT('Ctrl Pts',(-0.152484883621452,1.,2.00917680318426));
#25790=CARTESIAN_POINT('Ctrl Pts',(-0.150696157673084,-1.,2.01500291940243));
#25791=CARTESIAN_POINT('Ctrl Pts',(-0.150696157673084,1.,2.01500291940243));
#25792=CARTESIAN_POINT('Ctrl Pts',(-0.148856124775343,-1.,2.02083464969897));
#25793=CARTESIAN_POINT('Ctrl Pts',(-0.148856124775343,1.,2.02083464969897));
#25794=CARTESIAN_POINT('Ctrl Pts',(-0.146965557332586,-1.,2.02666926182017));
#25795=CARTESIAN_POINT('Ctrl Pts',(-0.146965557332586,1.,2.02666926182017));
#25796=CARTESIAN_POINT('Ctrl Pts',(-0.145025140186058,-1.,2.03250223739941));
#25797=CARTESIAN_POINT('Ctrl Pts',(-0.145025140186058,1.,2.03250223739941));
#25798=CARTESIAN_POINT('Ctrl Pts',(-0.143035515058208,-1.,2.03832911025913));
#25799=CARTESIAN_POINT('Ctrl Pts',(-0.143035515058208,1.,2.03832911025913));
#25800=CARTESIAN_POINT('Ctrl Pts',(-0.140997332152546,-1.,2.04414757947919));
#25801=CARTESIAN_POINT('Ctrl Pts',(-0.140997332152546,1.,2.04414757947919));
#25802=CARTESIAN_POINT('Ctrl Pts',(-0.138911255368966,-1.,2.04995762001333));
#25803=CARTESIAN_POINT('Ctrl Pts',(-0.138911255368966,1.,2.04995762001333));
#25804=CARTESIAN_POINT('Ctrl Pts',(-0.136777941218044,-1.,2.0557604441427));
#25805=CARTESIAN_POINT('Ctrl Pts',(-0.136777941218044,1.,2.0557604441427));
#25806=CARTESIAN_POINT('Ctrl Pts',(-0.134598026192107,-1.,2.06155781517844));
#25807=CARTESIAN_POINT('Ctrl Pts',(-0.134598026192107,1.,2.06155781517844));
#25808=CARTESIAN_POINT('Ctrl Pts',(-0.13237211154771,-1.,2.06735123910319));
#25809=CARTESIAN_POINT('Ctrl Pts',(-0.13237211154771,1.,2.06735123910319));
#25810=CARTESIAN_POINT('Ctrl Pts',(-0.130100748328401,-1.,2.07314114713047));
#25811=CARTESIAN_POINT('Ctrl Pts',(-0.130100748328401,1.,2.07314114713047));
#25812=CARTESIAN_POINT('Ctrl Pts',(-0.127784445276116,-1.,2.07892715110967));
#25813=CARTESIAN_POINT('Ctrl Pts',(-0.127784445276116,1.,2.07892715110967));
#25814=CARTESIAN_POINT('Ctrl Pts',(-0.125423679412058,-1.,2.08470840653628));
#25815=CARTESIAN_POINT('Ctrl Pts',(-0.125423679412058,1.,2.08470840653628));
#25816=CARTESIAN_POINT('Ctrl Pts',(-0.123018905621083,-1.,2.09048392424826));
#25817=CARTESIAN_POINT('Ctrl Pts',(-0.123018905621083,1.,2.09048392424826));
#25818=CARTESIAN_POINT('Ctrl Pts',(-0.120570567965129,-1.,2.09625292867756));
#25819=CARTESIAN_POINT('Ctrl Pts',(-0.120570567965129,1.,2.09625292867756));
#25820=CARTESIAN_POINT('Ctrl Pts',(-0.118079107988368,-1.,2.10201512132945));
#25821=CARTESIAN_POINT('Ctrl Pts',(-0.118079107988368,1.,2.10201512132945));
#25822=CARTESIAN_POINT('Ctrl Pts',(-0.115544957687941,-1.,2.10777050261359));
#25823=CARTESIAN_POINT('Ctrl Pts',(-0.115544957687941,1.,2.10777050261359));
#25824=CARTESIAN_POINT('Ctrl Pts',(-0.112968534419746,-1.,2.11351924490335));
#25825=CARTESIAN_POINT('Ctrl Pts',(-0.112968534419746,1.,2.11351924490335));
#25826=CARTESIAN_POINT('Ctrl Pts',(-0.11035023613502,-1.,2.11926155590849));
#25827=CARTESIAN_POINT('Ctrl Pts',(-0.11035023613502,1.,2.11926155590849));
#25828=CARTESIAN_POINT('Ctrl Pts',(-0.107690435231068,-1.,2.12499752306927));
#25829=CARTESIAN_POINT('Ctrl Pts',(-0.107690435231068,1.,2.12499752306927));
#25830=CARTESIAN_POINT('Ctrl Pts',(-0.104989479152703,-1.,2.1307270488718));
#25831=CARTESIAN_POINT('Ctrl Pts',(-0.104989479152703,1.,2.1307270488718));
#25832=CARTESIAN_POINT('Ctrl Pts',(-0.102247700556064,-1.,2.13644992667052));
#25833=CARTESIAN_POINT('Ctrl Pts',(-0.102247700556064,1.,2.13644992667052));
#25834=CARTESIAN_POINT('Ctrl Pts',(-0.0994654261990745,-1.,2.14216588395974));
#25835=CARTESIAN_POINT('Ctrl Pts',(-0.0994654261990745,1.,2.14216588395974));
#25836=CARTESIAN_POINT('Ctrl Pts',(-0.0966429852305691,-1.,2.14787463531864));
#25837=CARTESIAN_POINT('Ctrl Pts',(-0.0966429852305691,1.,2.14787463531864));
#25838=CARTESIAN_POINT('Ctrl Pts',(-0.0937807218868348,-1.,2.15357593978377));
#25839=CARTESIAN_POINT('Ctrl Pts',(-0.0937807218868348,1.,2.15357593978377));
#25840=CARTESIAN_POINT('Ctrl Pts',(-0.0908789888108269,-1.,2.15926961544808));
#25841=CARTESIAN_POINT('Ctrl Pts',(-0.0908789888108269,1.,2.15926961544808));
#25842=CARTESIAN_POINT('Ctrl Pts',(-0.0879381291387825,-1.,2.16495552645275));
#25843=CARTESIAN_POINT('Ctrl Pts',(-0.0879381291387825,1.,2.16495552645275));
#25844=CARTESIAN_POINT('Ctrl Pts',(-0.0849584620835646,-1.,2.17063357871031));
#25845=CARTESIAN_POINT('Ctrl Pts',(-0.0849584620835646,1.,2.17063357871031));
#25846=CARTESIAN_POINT('Ctrl Pts',(-0.0819402680871942,-1.,2.1763037121106));
#25847=CARTESIAN_POINT('Ctrl Pts',(-0.0819402680871942,1.,2.1763037121106));
#25848=CARTESIAN_POINT('Ctrl Pts',(-0.078883772768323,-1.,2.18196589448304));
#25849=CARTESIAN_POINT('Ctrl Pts',(-0.078883772768323,1.,2.18196589448304));
#25850=CARTESIAN_POINT('Ctrl Pts',(-0.0757891465833414,-1.,2.1876201139874));
#25851=CARTESIAN_POINT('Ctrl Pts',(-0.0757891465833414,1.,2.1876201139874));
#25852=CARTESIAN_POINT('Ctrl Pts',(-0.0732830357304279,-1.,2.19213712012956));
#25853=CARTESIAN_POINT('Ctrl Pts',(-0.0732830357304279,1.,2.19213712012956));
#25854=CARTESIAN_POINT('Ctrl Pts',(-0.071386377952463,-1.,2.19552129483562));
#25855=CARTESIAN_POINT('Ctrl Pts',(-0.071386377952463,1.,2.19552129483562));
#25856=CARTESIAN_POINT('Ctrl Pts',(-0.0701143536324929,-1.,2.19777582085261));
#25857=CARTESIAN_POINT('Ctrl Pts',(-0.0701143536324929,1.,2.19777582085261));
#25858=CARTESIAN_POINT('Ctrl Pts',(-0.0694764450219586,-1.,2.19890268624765));
#25859=CARTESIAN_POINT('Ctrl Pts',(-0.0694764450219586,1.,2.19890268624765));
#25860=CARTESIAN_POINT('',(-0.163289472382896,1.,1.74236521665491));
#25861=CARTESIAN_POINT('Ctrl Pts',(-0.163289472382896,1.,1.74236521665491));
#25862=CARTESIAN_POINT('Ctrl Pts',(-0.163814161002474,1.,1.74720349503904));
#25863=CARTESIAN_POINT('Ctrl Pts',(-0.164834765708484,1.,1.75666056640041));
#25864=CARTESIAN_POINT('Ctrl Pts',(-0.166279355148738,1.,1.77018771687692));
#25865=CARTESIAN_POINT('Ctrl Pts',(-0.16803277280837,1.,1.78690649988931));
#25866=CARTESIAN_POINT('Ctrl Pts',(-0.169936923908078,1.,1.80561530633924));
#25867=CARTESIAN_POINT('Ctrl Pts',(-0.171554770207306,1.,1.82215766815414));
#25868=CARTESIAN_POINT('Ctrl Pts',(-0.17288944289442,1.,1.83658380530747));
#25869=CARTESIAN_POINT('Ctrl Pts',(-0.173946627589401,1.,1.84898113200543));
#25870=CARTESIAN_POINT('Ctrl Pts',(-0.174735259276856,1.,1.85948367089838));
#25871=CARTESIAN_POINT('Ctrl Pts',(-0.175268337590901,1.,1.86828349694972));
#25872=CARTESIAN_POINT('Ctrl Pts',(-0.175563480746206,1.,1.87563767773249));
#25873=CARTESIAN_POINT('Ctrl Pts',(-0.175644148889271,1.,1.88188663144846));
#25874=CARTESIAN_POINT('Ctrl Pts',(-0.175538155840286,1.,1.88742606272818));
#25875=CARTESIAN_POINT('Ctrl Pts',(-0.175274276190664,1.,1.89264630198279));
#25876=CARTESIAN_POINT('Ctrl Pts',(-0.174879405091277,1.,1.89788101117148));
#25877=CARTESIAN_POINT('Ctrl Pts',(-0.174375518661222,1.,1.90335253863003));
#25878=CARTESIAN_POINT('Ctrl Pts',(-0.173776635257984,1.,1.90911693975475));
#25879=CARTESIAN_POINT('Ctrl Pts',(-0.173090695383619,1.,1.91511429159681));
#25880=CARTESIAN_POINT('Ctrl Pts',(-0.172321621259557,1.,1.92122334398034));
#25881=CARTESIAN_POINT('Ctrl Pts',(-0.17147119153296,1.,1.92731093582));
#25882=CARTESIAN_POINT('Ctrl Pts',(-0.170541253116136,1.,1.93329183155455));
#25883=CARTESIAN_POINT('Ctrl Pts',(-0.169534904817425,1.,1.93915639211497));
#25884=CARTESIAN_POINT('Ctrl Pts',(-0.168455741607516,1.,1.94493757756879));
#25885=CARTESIAN_POINT('Ctrl Pts',(-0.167307501784469,1.,1.95069027794286));
#25886=CARTESIAN_POINT('Ctrl Pts',(-0.166093592002833,1.,1.95646759718755));
#25887=CARTESIAN_POINT('Ctrl Pts',(-0.1648165689203,1.,1.96229379940174));
#25888=CARTESIAN_POINT('Ctrl Pts',(-0.16347818545776,1.,1.96816512678));
#25889=CARTESIAN_POINT('Ctrl Pts',(-0.162079693556302,1.,1.97406280235204));
#25890=CARTESIAN_POINT('Ctrl Pts',(-0.16062206078461,1.,1.97996195437557));
#25891=CARTESIAN_POINT('Ctrl Pts',(-0.159106226437289,1.,1.98584238283279));
#25892=CARTESIAN_POINT('Ctrl Pts',(-0.157533331459215,1.,1.99169810931893));
#25893=CARTESIAN_POINT('Ctrl Pts',(-0.155904629548775,1.,1.99753284771487));
#25894=CARTESIAN_POINT('Ctrl Pts',(-0.154221403049719,1.,2.00335565310539));
#25895=CARTESIAN_POINT('Ctrl Pts',(-0.152484883621452,1.,2.00917680318426));
#25896=CARTESIAN_POINT('Ctrl Pts',(-0.150696157673084,1.,2.01500291940243));
#25897=CARTESIAN_POINT('Ctrl Pts',(-0.148856124775343,1.,2.02083464969897));
#25898=CARTESIAN_POINT('Ctrl Pts',(-0.146965557332586,1.,2.02666926182017));
#25899=CARTESIAN_POINT('Ctrl Pts',(-0.145025140186058,1.,2.03250223739941));
#25900=CARTESIAN_POINT('Ctrl Pts',(-0.143035515058208,1.,2.03832911025913));
#25901=CARTESIAN_POINT('Ctrl Pts',(-0.140997332152546,1.,2.04414757947919));
#25902=CARTESIAN_POINT('Ctrl Pts',(-0.138911255368966,1.,2.04995762001333));
#25903=CARTESIAN_POINT('Ctrl Pts',(-0.136777941218044,1.,2.0557604441427));
#25904=CARTESIAN_POINT('Ctrl Pts',(-0.134598026192107,1.,2.06155781517844));
#25905=CARTESIAN_POINT('Ctrl Pts',(-0.13237211154771,1.,2.06735123910319));
#25906=CARTESIAN_POINT('Ctrl Pts',(-0.130100748328401,1.,2.07314114713047));
#25907=CARTESIAN_POINT('Ctrl Pts',(-0.127784445276116,1.,2.07892715110967));
#25908=CARTESIAN_POINT('Ctrl Pts',(-0.125423679412058,1.,2.08470840653628));
#25909=CARTESIAN_POINT('Ctrl Pts',(-0.123018905621083,1.,2.09048392424826));
#25910=CARTESIAN_POINT('Ctrl Pts',(-0.120570567965129,1.,2.09625292867756));
#25911=CARTESIAN_POINT('Ctrl Pts',(-0.118079107988368,1.,2.10201512132945));
#25912=CARTESIAN_POINT('Ctrl Pts',(-0.115544957687941,1.,2.10777050261359));
#25913=CARTESIAN_POINT('Ctrl Pts',(-0.112968534419746,1.,2.11351924490335));
#25914=CARTESIAN_POINT('Ctrl Pts',(-0.11035023613502,1.,2.11926155590849));
#25915=CARTESIAN_POINT('Ctrl Pts',(-0.107690435231068,1.,2.12499752306927));
#25916=CARTESIAN_POINT('Ctrl Pts',(-0.104989479152703,1.,2.1307270488718));
#25917=CARTESIAN_POINT('Ctrl Pts',(-0.102247700556064,1.,2.13644992667052));
#25918=CARTESIAN_POINT('Ctrl Pts',(-0.0994654261990745,1.,2.14216588395974));
#25919=CARTESIAN_POINT('Ctrl Pts',(-0.0966429852305691,1.,2.14787463531864));
#25920=CARTESIAN_POINT('Ctrl Pts',(-0.0937807218868348,1.,2.15357593978377));
#25921=CARTESIAN_POINT('Ctrl Pts',(-0.0908789888108269,1.,2.15926961544808));
#25922=CARTESIAN_POINT('Ctrl Pts',(-0.0879381291387825,1.,2.16495552645275));
#25923=CARTESIAN_POINT('Ctrl Pts',(-0.0849584620835646,1.,2.17063357871031));
#25924=CARTESIAN_POINT('Ctrl Pts',(-0.0819402680871942,1.,2.1763037121106));
#25925=CARTESIAN_POINT('Ctrl Pts',(-0.078883772768323,1.,2.18196589448304));
#25926=CARTESIAN_POINT('Ctrl Pts',(-0.0757891465833414,1.,2.1876201139874));
#25927=CARTESIAN_POINT('Ctrl Pts',(-0.0732830357304279,1.,2.19213712012956));
#25928=CARTESIAN_POINT('Ctrl Pts',(-0.071386377952463,1.,2.19552129483562));
#25929=CARTESIAN_POINT('Ctrl Pts',(-0.0701143536324929,1.,2.19777582085261));
#25930=CARTESIAN_POINT('Ctrl Pts',(-0.0694764450219586,1.,2.19890268624765));
#25931=CARTESIAN_POINT('',(-0.163289472382897,0.,1.74236521665491));
#25932=CARTESIAN_POINT('Origin',(0.,0.,0.));
#25933=CARTESIAN_POINT('',(-0.383122945602004,1.,1.7075470150345));
#25934=CARTESIAN_POINT('Origin',(0.,1.,0.));
#25935=CARTESIAN_POINT('',(-0.383122945602004,0.,1.7075470150345));
#25936=CARTESIAN_POINT('Ctrl Pts',(-0.61342227326009,-1.,2.11275013067528));
#25937=CARTESIAN_POINT('Ctrl Pts',(-0.61342227326009,1.,2.11275013067528));
#25938=CARTESIAN_POINT('Ctrl Pts',(-0.61246736556225,-1.,2.11187554260142));
#25939=CARTESIAN_POINT('Ctrl Pts',(-0.61246736556225,1.,2.11187554260142));
#25940=CARTESIAN_POINT('Ctrl Pts',(-0.610560911691113,-1.,2.11012443807661));
#25941=CARTESIAN_POINT('Ctrl Pts',(-0.610560911691113,1.,2.11012443807661));
#25942=CARTESIAN_POINT('Ctrl Pts',(-0.607711315456826,-1.,2.10749199615859));
#25943=CARTESIAN_POINT('Ctrl Pts',(-0.607711315456826,1.,2.10749199615859));
#25944=CARTESIAN_POINT('Ctrl Pts',(-0.603932030738212,-1.,2.10397049887709));
#25945=CARTESIAN_POINT('Ctrl Pts',(-0.603932030738212,1.,2.10397049887709));
#25946=CARTESIAN_POINT('Ctrl Pts',(-0.599241616422144,-1.,2.09954930865331));
#25947=CARTESIAN_POINT('Ctrl Pts',(-0.599241616422144,1.,2.09954930865331));
#25948=CARTESIAN_POINT('Ctrl Pts',(-0.594585006052824,-1.,2.09510876220501));
#25949=CARTESIAN_POINT('Ctrl Pts',(-0.594585006052824,1.,2.09510876220501));
#25950=CARTESIAN_POINT('Ctrl Pts',(-0.589962365403189,-1.,2.09064881812053));
#25951=CARTESIAN_POINT('Ctrl Pts',(-0.589962365403189,1.,2.09064881812053));
#25952=CARTESIAN_POINT('Ctrl Pts',(-0.585373918990895,-1.,2.086169437277));
#25953=CARTESIAN_POINT('Ctrl Pts',(-0.585373918990895,1.,2.086169437277));
#25954=CARTESIAN_POINT('Ctrl Pts',(-0.580819952107257,-1.,2.08167059018138));
#25955=CARTESIAN_POINT('Ctrl Pts',(-0.580819952107257,1.,2.08167059018138));
#25956=CARTESIAN_POINT('Ctrl Pts',(-0.576300797416275,-1.,2.07715226767361));
#25957=CARTESIAN_POINT('Ctrl Pts',(-0.576300797416275,1.,2.07715226767361));
#25958=CARTESIAN_POINT('Ctrl Pts',(-0.571816823242411,-1.,2.07261449292757));
#25959=CARTESIAN_POINT('Ctrl Pts',(-0.571816823242411,1.,2.07261449292757));
#25960=CARTESIAN_POINT('Ctrl Pts',(-0.567368421181229,-1.,2.06805732997383));
#25961=CARTESIAN_POINT('Ctrl Pts',(-0.567368421181229,1.,2.06805732997383));
#25962=CARTESIAN_POINT('Ctrl Pts',(-0.562955993082574,-1.,2.06348090160697));
#25963=CARTESIAN_POINT('Ctrl Pts',(-0.562955993082574,1.,2.06348090160697));
#25964=CARTESIAN_POINT('Ctrl Pts',(-0.558579940185467,-1.,2.05888537756571));
#25965=CARTESIAN_POINT('Ctrl Pts',(-0.558579940185467,1.,2.05888537756571));
#25966=CARTESIAN_POINT('Ctrl Pts',(-0.55424065746411,-1.,2.05427091604482));
#25967=CARTESIAN_POINT('Ctrl Pts',(-0.55424065746411,1.,2.05427091604482));
#25968=CARTESIAN_POINT('Ctrl Pts',(-0.549938525150342,-1.,2.04963761077974));
#25969=CARTESIAN_POINT('Ctrl Pts',(-0.549938525150342,1.,2.04963761077974));
#25970=CARTESIAN_POINT('Ctrl Pts',(-0.545673903817348,-1.,2.0449854471456));
#25971=CARTESIAN_POINT('Ctrl Pts',(-0.545673903817348,1.,2.0449854471456));
#25972=CARTESIAN_POINT('Ctrl Pts',(-0.54144712061552,-1.,2.0403142269048));
#25973=CARTESIAN_POINT('Ctrl Pts',(-0.54144712061552,1.,2.0403142269048));
#25974=CARTESIAN_POINT('Ctrl Pts',(-0.537258489833134,-1.,2.03562362953993));
#25975=CARTESIAN_POINT('Ctrl Pts',(-0.537258489833134,1.,2.03562362953993));
#25976=CARTESIAN_POINT('Ctrl Pts',(-0.533108355132905,-1.,2.03091336214401));
#25977=CARTESIAN_POINT('Ctrl Pts',(-0.533108355132905,1.,2.03091336214401));
#25978=CARTESIAN_POINT('Ctrl Pts',(-0.528997127241911,-1.,2.02618329083289));
#25979=CARTESIAN_POINT('Ctrl Pts',(-0.528997127241911,1.,2.02618329083289));
#25980=CARTESIAN_POINT('Ctrl Pts',(-0.524925318333518,-1.,2.02143356304712));
#25981=CARTESIAN_POINT('Ctrl Pts',(-0.524925318333518,1.,2.02143356304712));
#25982=CARTESIAN_POINT('Ctrl Pts',(-0.520893590399428,-1.,2.01666477917305));
#25983=CARTESIAN_POINT('Ctrl Pts',(-0.520893590399428,1.,2.01666477917305));
#25984=CARTESIAN_POINT('Ctrl Pts',(-0.516902681728733,-1.,2.01187773939257));
#25985=CARTESIAN_POINT('Ctrl Pts',(-0.516902681728733,1.,2.01187773939257));
#25986=CARTESIAN_POINT('Ctrl Pts',(-0.512953306961814,-1.,2.00707309946955));
#25987=CARTESIAN_POINT('Ctrl Pts',(-0.512953306961814,1.,2.00707309946955));
#25988=CARTESIAN_POINT('Ctrl Pts',(-0.509046069886152,-1.,2.00225107134733));
#25989=CARTESIAN_POINT('Ctrl Pts',(-0.509046069886152,1.,2.00225107134733));
#25990=CARTESIAN_POINT('Ctrl Pts',(-0.505181361323011,-1.,1.99741107463567));
#25991=CARTESIAN_POINT('Ctrl Pts',(-0.505181361323011,1.,1.99741107463567));
#25992=CARTESIAN_POINT('Ctrl Pts',(-0.501359287727129,-1.,1.9925514912615));
#25993=CARTESIAN_POINT('Ctrl Pts',(-0.501359287727129,1.,1.9925514912615));
#25994=CARTESIAN_POINT('Ctrl Pts',(-0.497579909545564,-1.,1.98767044752929));
#25995=CARTESIAN_POINT('Ctrl Pts',(-0.497579909545564,1.,1.98767044752929));
#25996=CARTESIAN_POINT('Ctrl Pts',(-0.493843476541492,-1.,1.9827665876182));
#25997=CARTESIAN_POINT('Ctrl Pts',(-0.493843476541492,1.,1.9827665876182));
#25998=CARTESIAN_POINT('Ctrl Pts',(-0.490150627860955,-1.,1.97783973019229));
#25999=CARTESIAN_POINT('Ctrl Pts',(-0.490150627860955,1.,1.97783973019229));
#26000=CARTESIAN_POINT('Ctrl Pts',(-0.486502692907661,-1.,1.97289186263272));
#26001=CARTESIAN_POINT('Ctrl Pts',(-0.486502692907661,1.,1.97289186263272));
#26002=CARTESIAN_POINT('Ctrl Pts',(-0.482901662120687,-1.,1.96792703422358));
#26003=CARTESIAN_POINT('Ctrl Pts',(-0.482901662120687,1.,1.96792703422358));
#26004=CARTESIAN_POINT('Ctrl Pts',(-0.479349583074846,-1.,1.96294933055938));
#26005=CARTESIAN_POINT('Ctrl Pts',(-0.479349583074846,1.,1.96294933055938));
#26006=CARTESIAN_POINT('Ctrl Pts',(-0.475848034683172,-1.,1.95796111148175));
#26007=CARTESIAN_POINT('Ctrl Pts',(-0.475848034683172,1.,1.95796111148175));
#26008=CARTESIAN_POINT('Ctrl Pts',(-0.47239767226408,-1.,1.95296148278136));
#26009=CARTESIAN_POINT('Ctrl Pts',(-0.47239767226408,1.,1.95296148278136));
#26010=CARTESIAN_POINT('Ctrl Pts',(-0.468997482913158,-1.,1.94794381136524));
#26011=CARTESIAN_POINT('Ctrl Pts',(-0.468997482913158,1.,1.94794381136524));
#26012=CARTESIAN_POINT('Ctrl Pts',(-0.465645462026065,-1.,1.94289794196205));
#26013=CARTESIAN_POINT('Ctrl Pts',(-0.465645462026065,1.,1.94289794196205));
#26014=CARTESIAN_POINT('Ctrl Pts',(-0.462340031009087,-1.,1.93781486640834));
#26015=CARTESIAN_POINT('Ctrl Pts',(-0.462340031009087,1.,1.93781486640834));
#26016=CARTESIAN_POINT('Ctrl Pts',(-0.459081234547931,-1.,1.93269066517936));
#26017=CARTESIAN_POINT('Ctrl Pts',(-0.459081234547931,1.,1.93269066517936));
#26018=CARTESIAN_POINT('Ctrl Pts',(-0.455872005174335,-1.,1.92753067150461));
#26019=CARTESIAN_POINT('Ctrl Pts',(-0.455872005174335,1.,1.92753067150461));
#26020=CARTESIAN_POINT('Ctrl Pts',(-0.452719478359356,-1.,1.9223538064847));
#26021=CARTESIAN_POINT('Ctrl Pts',(-0.452719478359356,1.,1.9223538064847));
#26022=CARTESIAN_POINT('Ctrl Pts',(-0.449632260106572,-1.,1.91718342555717));
#26023=CARTESIAN_POINT('Ctrl Pts',(-0.449632260106572,1.,1.91718342555717));
#26024=CARTESIAN_POINT('Ctrl Pts',(-0.446617343485651,-1.,1.91203699981095));
#26025=CARTESIAN_POINT('Ctrl Pts',(-0.446617343485651,1.,1.91203699981095));
#26026=CARTESIAN_POINT('Ctrl Pts',(-0.44367755684917,-1.,1.90691756144906));
#26027=CARTESIAN_POINT('Ctrl Pts',(-0.44367755684917,1.,1.90691756144906));
#26028=CARTESIAN_POINT('Ctrl Pts',(-0.440807833704161,-1.,1.90180124389137));
#26029=CARTESIAN_POINT('Ctrl Pts',(-0.440807833704161,1.,1.90180124389137));
#26030=CARTESIAN_POINT('Ctrl Pts',(-0.437995003948443,-1.,1.89663648956549));
#26031=CARTESIAN_POINT('Ctrl Pts',(-0.437995003948443,1.,1.89663648956549));
#26032=CARTESIAN_POINT('Ctrl Pts',(-0.43522566096358,-1.,1.89136993975585));
#26033=CARTESIAN_POINT('Ctrl Pts',(-0.43522566096358,1.,1.89136993975585));
#26034=CARTESIAN_POINT('Ctrl Pts',(-0.432493038548833,-1.,1.88596913666828));
#26035=CARTESIAN_POINT('Ctrl Pts',(-0.432493038548833,1.,1.88596913666828));
#26036=CARTESIAN_POINT('Ctrl Pts',(-0.429803062482217,-1.,1.88044229001778));
#26037=CARTESIAN_POINT('Ctrl Pts',(-0.429803062482217,1.,1.88044229001778));
#26038=CARTESIAN_POINT('Ctrl Pts',(-0.427183828518743,-1.,1.87486989291333));
#26039=CARTESIAN_POINT('Ctrl Pts',(-0.427183828518743,1.,1.87486989291333));
#26040=CARTESIAN_POINT('Ctrl Pts',(-0.424678177290876,-1.,1.8693780394412));
#26041=CARTESIAN_POINT('Ctrl Pts',(-0.424678177290876,1.,1.8693780394412));
#26042=CARTESIAN_POINT('Ctrl Pts',(-0.422327307417885,-1.,1.86408083333863));
#26043=CARTESIAN_POINT('Ctrl Pts',(-0.422327307417885,1.,1.86408083333863));
#26044=CARTESIAN_POINT('Ctrl Pts',(-0.420157287975583,-1.,1.8590328109667));
#26045=CARTESIAN_POINT('Ctrl Pts',(-0.420157287975583,1.,1.8590328109667));
#26046=CARTESIAN_POINT('Ctrl Pts',(-0.418164129144045,-1.,1.8541763285645));
#26047=CARTESIAN_POINT('Ctrl Pts',(-0.418164129144045,1.,1.8541763285645));
#26048=CARTESIAN_POINT('Ctrl Pts',(-0.416300022039885,-1.,1.84929312930314));
#26049=CARTESIAN_POINT('Ctrl Pts',(-0.416300022039885,1.,1.84929312930314));
#26050=CARTESIAN_POINT('Ctrl Pts',(-0.414487438255542,-1.,1.84405757074218));
#26051=CARTESIAN_POINT('Ctrl Pts',(-0.414487438255542,1.,1.84405757074218));
#26052=CARTESIAN_POINT('Ctrl Pts',(-0.412633125322945,-1.,1.8380895347617));
#26053=CARTESIAN_POINT('Ctrl Pts',(-0.412633125322945,1.,1.8380895347617));
#26054=CARTESIAN_POINT('Ctrl Pts',(-0.410641256301276,-1.,1.83100408895047));
#26055=CARTESIAN_POINT('Ctrl Pts',(-0.410641256301276,1.,1.83100408895047));
#26056=CARTESIAN_POINT('Ctrl Pts',(-0.408428948106227,-1.,1.82247022677562));
#26057=CARTESIAN_POINT('Ctrl Pts',(-0.408428948106227,1.,1.82247022677562));
#26058=CARTESIAN_POINT('Ctrl Pts',(-0.405933518407175,-1.,1.81223801812013));
#26059=CARTESIAN_POINT('Ctrl Pts',(-0.405933518407175,1.,1.81223801812013));
#26060=CARTESIAN_POINT('Ctrl Pts',(-0.403107976163396,-1.,1.80012077173238));
#26061=CARTESIAN_POINT('Ctrl Pts',(-0.403107976163396,1.,1.80012077173238));
#26062=CARTESIAN_POINT('Ctrl Pts',(-0.399919403774155,-1.,1.78598826343754));
#26063=CARTESIAN_POINT('Ctrl Pts',(-0.399919403774155,1.,1.78598826343754));
#26064=CARTESIAN_POINT('Ctrl Pts',(-0.396346196110688,-1.,1.76975560043442));
#26065=CARTESIAN_POINT('Ctrl Pts',(-0.396346196110688,1.,1.76975560043442));
#26066=CARTESIAN_POINT('Ctrl Pts',(-0.392375812285395,-1.,1.75137405310193));
#26067=CARTESIAN_POINT('Ctrl Pts',(-0.392375812285395,1.,1.75137405310193));
#26068=CARTESIAN_POINT('Ctrl Pts',(-0.388877023502615,-1.,1.73493170972829));
#26069=CARTESIAN_POINT('Ctrl Pts',(-0.388877023502615,1.,1.73493170972829));
#26070=CARTESIAN_POINT('Ctrl Pts',(-0.386070790323281,-1.,1.72162022244582));
#26071=CARTESIAN_POINT('Ctrl Pts',(-0.386070790323281,1.,1.72162022244582));
#26072=CARTESIAN_POINT('Ctrl Pts',(-0.384119047314215,-1.,1.71231062891398));
#26073=CARTESIAN_POINT('Ctrl Pts',(-0.384119047314215,1.,1.71231062891398));
#26074=CARTESIAN_POINT('Ctrl Pts',(-0.383122945602004,-1.,1.7075470150345));
#26075=CARTESIAN_POINT('Ctrl Pts',(-0.383122945602004,1.,1.7075470150345));
#26076=CARTESIAN_POINT('',(-0.61342227326009,1.,2.11275013067528));
#26077=CARTESIAN_POINT('Ctrl Pts',(-0.61342227326009,1.,2.11275013067528));
#26078=CARTESIAN_POINT('Ctrl Pts',(-0.61246736556225,1.,2.11187554260142));
#26079=CARTESIAN_POINT('Ctrl Pts',(-0.610560911691113,1.,2.11012443807661));
#26080=CARTESIAN_POINT('Ctrl Pts',(-0.607711315456826,1.,2.10749199615859));
#26081=CARTESIAN_POINT('Ctrl Pts',(-0.603932030738212,1.,2.10397049887709));
#26082=CARTESIAN_POINT('Ctrl Pts',(-0.599241616422144,1.,2.09954930865331));
#26083=CARTESIAN_POINT('Ctrl Pts',(-0.594585006052824,1.,2.09510876220501));
#26084=CARTESIAN_POINT('Ctrl Pts',(-0.589962365403189,1.,2.09064881812053));
#26085=CARTESIAN_POINT('Ctrl Pts',(-0.585373918990895,1.,2.086169437277));
#26086=CARTESIAN_POINT('Ctrl Pts',(-0.580819952107257,1.,2.08167059018138));
#26087=CARTESIAN_POINT('Ctrl Pts',(-0.576300797416275,1.,2.07715226767361));
#26088=CARTESIAN_POINT('Ctrl Pts',(-0.571816823242411,1.,2.07261449292757));
#26089=CARTESIAN_POINT('Ctrl Pts',(-0.567368421181229,1.,2.06805732997383));
#26090=CARTESIAN_POINT('Ctrl Pts',(-0.562955993082574,1.,2.06348090160697));
#26091=CARTESIAN_POINT('Ctrl Pts',(-0.558579940185467,1.,2.05888537756571));
#26092=CARTESIAN_POINT('Ctrl Pts',(-0.55424065746411,1.,2.05427091604482));
#26093=CARTESIAN_POINT('Ctrl Pts',(-0.549938525150342,1.,2.04963761077974));
#26094=CARTESIAN_POINT('Ctrl Pts',(-0.545673903817348,1.,2.0449854471456));
#26095=CARTESIAN_POINT('Ctrl Pts',(-0.54144712061552,1.,2.0403142269048));
#26096=CARTESIAN_POINT('Ctrl Pts',(-0.537258489833134,1.,2.03562362953993));
#26097=CARTESIAN_POINT('Ctrl Pts',(-0.533108355132905,1.,2.03091336214401));
#26098=CARTESIAN_POINT('Ctrl Pts',(-0.528997127241911,1.,2.02618329083289));
#26099=CARTESIAN_POINT('Ctrl Pts',(-0.524925318333518,1.,2.02143356304712));
#26100=CARTESIAN_POINT('Ctrl Pts',(-0.520893590399428,1.,2.01666477917305));
#26101=CARTESIAN_POINT('Ctrl Pts',(-0.516902681728733,1.,2.01187773939257));
#26102=CARTESIAN_POINT('Ctrl Pts',(-0.512953306961814,1.,2.00707309946955));
#26103=CARTESIAN_POINT('Ctrl Pts',(-0.509046069886152,1.,2.00225107134733));
#26104=CARTESIAN_POINT('Ctrl Pts',(-0.505181361323011,1.,1.99741107463567));
#26105=CARTESIAN_POINT('Ctrl Pts',(-0.501359287727129,1.,1.9925514912615));
#26106=CARTESIAN_POINT('Ctrl Pts',(-0.497579909545564,1.,1.98767044752929));
#26107=CARTESIAN_POINT('Ctrl Pts',(-0.493843476541492,1.,1.9827665876182));
#26108=CARTESIAN_POINT('Ctrl Pts',(-0.490150627860955,1.,1.97783973019229));
#26109=CARTESIAN_POINT('Ctrl Pts',(-0.486502692907661,1.,1.97289186263272));
#26110=CARTESIAN_POINT('Ctrl Pts',(-0.482901662120687,1.,1.96792703422358));
#26111=CARTESIAN_POINT('Ctrl Pts',(-0.479349583074846,1.,1.96294933055938));
#26112=CARTESIAN_POINT('Ctrl Pts',(-0.475848034683172,1.,1.95796111148175));
#26113=CARTESIAN_POINT('Ctrl Pts',(-0.47239767226408,1.,1.95296148278136));
#26114=CARTESIAN_POINT('Ctrl Pts',(-0.468997482913158,1.,1.94794381136524));
#26115=CARTESIAN_POINT('Ctrl Pts',(-0.465645462026065,1.,1.94289794196205));
#26116=CARTESIAN_POINT('Ctrl Pts',(-0.462340031009087,1.,1.93781486640834));
#26117=CARTESIAN_POINT('Ctrl Pts',(-0.459081234547931,1.,1.93269066517936));
#26118=CARTESIAN_POINT('Ctrl Pts',(-0.455872005174335,1.,1.92753067150461));
#26119=CARTESIAN_POINT('Ctrl Pts',(-0.452719478359356,1.,1.9223538064847));
#26120=CARTESIAN_POINT('Ctrl Pts',(-0.449632260106572,1.,1.91718342555717));
#26121=CARTESIAN_POINT('Ctrl Pts',(-0.446617343485651,1.,1.91203699981095));
#26122=CARTESIAN_POINT('Ctrl Pts',(-0.44367755684917,1.,1.90691756144906));
#26123=CARTESIAN_POINT('Ctrl Pts',(-0.440807833704161,1.,1.90180124389137));
#26124=CARTESIAN_POINT('Ctrl Pts',(-0.437995003948443,1.,1.89663648956549));
#26125=CARTESIAN_POINT('Ctrl Pts',(-0.43522566096358,1.,1.89136993975585));
#26126=CARTESIAN_POINT('Ctrl Pts',(-0.432493038548833,1.,1.88596913666828));
#26127=CARTESIAN_POINT('Ctrl Pts',(-0.429803062482217,1.,1.88044229001778));
#26128=CARTESIAN_POINT('Ctrl Pts',(-0.427183828518743,1.,1.87486989291333));
#26129=CARTESIAN_POINT('Ctrl Pts',(-0.424678177290876,1.,1.8693780394412));
#26130=CARTESIAN_POINT('Ctrl Pts',(-0.422327307417885,1.,1.86408083333863));
#26131=CARTESIAN_POINT('Ctrl Pts',(-0.420157287975583,1.,1.8590328109667));
#26132=CARTESIAN_POINT('Ctrl Pts',(-0.418164129144045,1.,1.8541763285645));
#26133=CARTESIAN_POINT('Ctrl Pts',(-0.416300022039885,1.,1.84929312930314));
#26134=CARTESIAN_POINT('Ctrl Pts',(-0.414487438255542,1.,1.84405757074218));
#26135=CARTESIAN_POINT('Ctrl Pts',(-0.412633125322945,1.,1.8380895347617));
#26136=CARTESIAN_POINT('Ctrl Pts',(-0.410641256301276,1.,1.83100408895047));
#26137=CARTESIAN_POINT('Ctrl Pts',(-0.408428948106227,1.,1.82247022677562));
#26138=CARTESIAN_POINT('Ctrl Pts',(-0.405933518407175,1.,1.81223801812013));
#26139=CARTESIAN_POINT('Ctrl Pts',(-0.403107976163396,1.,1.80012077173238));
#26140=CARTESIAN_POINT('Ctrl Pts',(-0.399919403774155,1.,1.78598826343754));
#26141=CARTESIAN_POINT('Ctrl Pts',(-0.396346196110688,1.,1.76975560043442));
#26142=CARTESIAN_POINT('Ctrl Pts',(-0.392375812285395,1.,1.75137405310193));
#26143=CARTESIAN_POINT('Ctrl Pts',(-0.388877023502615,1.,1.73493170972829));
#26144=CARTESIAN_POINT('Ctrl Pts',(-0.386070790323281,1.,1.72162022244582));
#26145=CARTESIAN_POINT('Ctrl Pts',(-0.384119047314215,1.,1.71231062891398));
#26146=CARTESIAN_POINT('Ctrl Pts',(-0.383122945602004,1.,1.7075470150345));
#26147=CARTESIAN_POINT('',(-0.61342227326009,0.,2.11275013067528));
#26148=CARTESIAN_POINT('Origin',(-0.745574324794401,0.,2.0698113262342));
#26149=CARTESIAN_POINT('',(-0.745574324794401,1.,2.0698113262342));
#26150=CARTESIAN_POINT('',(-0.61342227326009,1.,2.11275013067528));
#26151=CARTESIAN_POINT('',(-0.745574324794401,0.,2.0698113262342));
#26152=CARTESIAN_POINT('Ctrl Pts',(-0.693717979106306,-1.,1.60662857109684));
#26153=CARTESIAN_POINT('Ctrl Pts',(-0.693717979106306,1.,1.60662857109684));
#26154=CARTESIAN_POINT('Ctrl Pts',(-0.695712097881194,-1.,1.61106790958151));
#26155=CARTESIAN_POINT('Ctrl Pts',(-0.695712097881194,1.,1.61106790958151));
#26156=CARTESIAN_POINT('Ctrl Pts',(-0.699605146405088,-1.,1.61974673472612));
#26157=CARTESIAN_POINT('Ctrl Pts',(-0.699605146405088,1.,1.61974673472612));
#26158=CARTESIAN_POINT('Ctrl Pts',(-0.705159151988319,-1.,1.63216541664676));
#26159=CARTESIAN_POINT('Ctrl Pts',(-0.705159151988319,1.,1.63216541664676));
#26160=CARTESIAN_POINT('Ctrl Pts',(-0.711993139355394,-1.,1.64752408832016));
#26161=CARTESIAN_POINT('Ctrl Pts',(-0.711993139355394,1.,1.64752408832016));
#26162=CARTESIAN_POINT('Ctrl Pts',(-0.719585433804282,-1.,1.6647288055568));
#26163=CARTESIAN_POINT('Ctrl Pts',(-0.719585433804282,1.,1.6647288055568));
#26164=CARTESIAN_POINT('Ctrl Pts',(-0.726235967997433,-1.,1.67996158455503));
#26165=CARTESIAN_POINT('Ctrl Pts',(-0.726235967997433,1.,1.67996158455503));
#26166=CARTESIAN_POINT('Ctrl Pts',(-0.731963238697195,-1.,1.69326921975743));
#26167=CARTESIAN_POINT('Ctrl Pts',(-0.731963238697195,1.,1.69326921975743));
#26168=CARTESIAN_POINT('Ctrl Pts',(-0.736799665724771,-1.,1.70473309006121));
#26169=CARTESIAN_POINT('Ctrl Pts',(-0.736799665724771,1.,1.70473309006121));
#26170=CARTESIAN_POINT('Ctrl Pts',(-0.740795162032088,-1.,1.71447789751927));
#26171=CARTESIAN_POINT('Ctrl Pts',(-0.740795162032088,1.,1.71447789751927));
#26172=CARTESIAN_POINT('Ctrl Pts',(-0.744021445433764,-1.,1.7226822991693));
#26173=CARTESIAN_POINT('Ctrl Pts',(-0.744021445433764,1.,1.7226822991693));
#26174=CARTESIAN_POINT('Ctrl Pts',(-0.746574710096436,-1.,1.72958533647399));
#26175=CARTESIAN_POINT('Ctrl Pts',(-0.746574710096436,1.,1.72958533647399));
#26176=CARTESIAN_POINT('Ctrl Pts',(-0.748582462954855,-1.,1.73550351679848));
#26177=CARTESIAN_POINT('Ctrl Pts',(-0.748582462954855,1.,1.73550351679848));
#26178=CARTESIAN_POINT('Ctrl Pts',(-0.75019343597954,-1.,1.74080458266705));
#26179=CARTESIAN_POINT('Ctrl Pts',(-0.75019343597954,1.,1.74080458266705));
#26180=CARTESIAN_POINT('Ctrl Pts',(-0.751555614163629,-1.,1.74585086852298));
#26181=CARTESIAN_POINT('Ctrl Pts',(-0.751555614163629,1.,1.74585086852298));
#26182=CARTESIAN_POINT('Ctrl Pts',(-0.752797683531377,-1.,1.75095139468809));
#26183=CARTESIAN_POINT('Ctrl Pts',(-0.752797683531377,1.,1.75095139468809));
#26184=CARTESIAN_POINT('Ctrl Pts',(-0.75400925402848,-1.,1.75631083600175));
#26185=CARTESIAN_POINT('Ctrl Pts',(-0.75400925402848,1.,1.75631083600175));
#26186=CARTESIAN_POINT('Ctrl Pts',(-0.755220979975262,-1.,1.7619781724032));
#26187=CARTESIAN_POINT('Ctrl Pts',(-0.755220979975262,1.,1.7619781724032));
#26188=CARTESIAN_POINT('Ctrl Pts',(-0.756421896028403,-1.,1.76789396003141));
#26189=CARTESIAN_POINT('Ctrl Pts',(-0.756421896028403,1.,1.76789396003141));
#26190=CARTESIAN_POINT('Ctrl Pts',(-0.757578264077238,-1.,1.77394167108342));
#26191=CARTESIAN_POINT('Ctrl Pts',(-0.757578264077238,1.,1.77394167108342));
#26192=CARTESIAN_POINT('Ctrl Pts',(-0.75865062667738,-1.,1.77999411220912));
#26193=CARTESIAN_POINT('Ctrl Pts',(-0.75865062667738,1.,1.77999411220912));
#26194=CARTESIAN_POINT('Ctrl Pts',(-0.759614401109868,-1.,1.78596964884526));
#26195=CARTESIAN_POINT('Ctrl Pts',(-0.759614401109868,1.,1.78596964884526));
#26196=CARTESIAN_POINT('Ctrl Pts',(-0.760469555880425,-1.,1.79185815610802));
#26197=CARTESIAN_POINT('Ctrl Pts',(-0.760469555880425,1.,1.79185815610802));
#26198=CARTESIAN_POINT('Ctrl Pts',(-0.761229695230359,-1.,1.79768986997735));
#26199=CARTESIAN_POINT('Ctrl Pts',(-0.761229695230359,1.,1.79768986997735));
#26200=CARTESIAN_POINT('Ctrl Pts',(-0.761915336443516,-1.,1.80351583877334));
#26201=CARTESIAN_POINT('Ctrl Pts',(-0.761915336443516,1.,1.80351583877334));
#26202=CARTESIAN_POINT('Ctrl Pts',(-0.762546129464036,-1.,1.80938551463989));
#26203=CARTESIAN_POINT('Ctrl Pts',(-0.762546129464036,1.,1.80938551463989));
#26204=CARTESIAN_POINT('Ctrl Pts',(-0.763132003836783,-1.,1.81532118405566));
#26205=CARTESIAN_POINT('Ctrl Pts',(-0.763132003836783,1.,1.81532118405566));
#26206=CARTESIAN_POINT('Ctrl Pts',(-0.763673465462854,-1.,1.82131873145297));
#26207=CARTESIAN_POINT('Ctrl Pts',(-0.763673465462854,1.,1.82131873145297));
#26208=CARTESIAN_POINT('Ctrl Pts',(-0.764165902606055,-1.,1.8273599120008));
#26209=CARTESIAN_POINT('Ctrl Pts',(-0.764165902606055,1.,1.8273599120008));
#26210=CARTESIAN_POINT('Ctrl Pts',(-0.764602549687845,-1.,1.8334207722714));
#26211=CARTESIAN_POINT('Ctrl Pts',(-0.764602549687845,1.,1.8334207722714));
#26212=CARTESIAN_POINT('Ctrl Pts',(-0.764978057881687,-1.,1.83948181064823));
#26213=CARTESIAN_POINT('Ctrl Pts',(-0.764978057881687,1.,1.83948181064823));
#26214=CARTESIAN_POINT('Ctrl Pts',(-0.765291664861971,-1.,1.8455369887591));
#26215=CARTESIAN_POINT('Ctrl Pts',(-0.765291664861971,1.,1.8455369887591));
#26216=CARTESIAN_POINT('Ctrl Pts',(-0.765545710619023,-1.,1.85158945130054));
#26217=CARTESIAN_POINT('Ctrl Pts',(-0.765545710619023,1.,1.85158945130054));
#26218=CARTESIAN_POINT('Ctrl Pts',(-0.765744212909305,-1.,1.85764741390391));
#26219=CARTESIAN_POINT('Ctrl Pts',(-0.765744212909305,1.,1.85764741390391));
#26220=CARTESIAN_POINT('Ctrl Pts',(-0.765891519092557,-1.,1.86372027063314));
#26221=CARTESIAN_POINT('Ctrl Pts',(-0.765891519092557,1.,1.86372027063314));
#26222=CARTESIAN_POINT('Ctrl Pts',(-0.765990708546111,-1.,1.86981398314345));
#26223=CARTESIAN_POINT('Ctrl Pts',(-0.765990708546111,1.,1.86981398314345));
#26224=CARTESIAN_POINT('Ctrl Pts',(-0.766042837036759,-1.,1.87592888967886));
#26225=CARTESIAN_POINT('Ctrl Pts',(-0.766042837036759,1.,1.87592888967886));
#26226=CARTESIAN_POINT('Ctrl Pts',(-0.766047794851869,-1.,1.88206215302561));
#26227=CARTESIAN_POINT('Ctrl Pts',(-0.766047794851869,1.,1.88206215302561));
#26228=CARTESIAN_POINT('Ctrl Pts',(-0.76600483706209,-1.,1.88820926433409));
#26229=CARTESIAN_POINT('Ctrl Pts',(-0.76600483706209,1.,1.88820926433409));
#26230=CARTESIAN_POINT('Ctrl Pts',(-0.765913193856979,-1.,1.89436577771389));
#26231=CARTESIAN_POINT('Ctrl Pts',(-0.765913193856979,1.,1.89436577771389));
#26232=CARTESIAN_POINT('Ctrl Pts',(-0.765772772593395,-1.,1.90052930393599));
#26233=CARTESIAN_POINT('Ctrl Pts',(-0.765772772593395,1.,1.90052930393599));
#26234=CARTESIAN_POINT('Ctrl Pts',(-0.765584196937936,-1.,1.90669961402362));
#26235=CARTESIAN_POINT('Ctrl Pts',(-0.765584196937936,1.,1.90669961402362));
#26236=CARTESIAN_POINT('Ctrl Pts',(-0.765348465884739,-1.,1.91287765805174));
#26237=CARTESIAN_POINT('Ctrl Pts',(-0.765348465884739,1.,1.91287765805174));
#26238=CARTESIAN_POINT('Ctrl Pts',(-0.765066729667095,-1.,1.91906491634197));
#26239=CARTESIAN_POINT('Ctrl Pts',(-0.765066729667095,1.,1.91906491634197));
#26240=CARTESIAN_POINT('Ctrl Pts',(-0.764740025488189,-1.,1.92526263537041));
#26241=CARTESIAN_POINT('Ctrl Pts',(-0.764740025488189,1.,1.92526263537041));
#26242=CARTESIAN_POINT('Ctrl Pts',(-0.764369010673889,-1.,1.93147105496367));
#26243=CARTESIAN_POINT('Ctrl Pts',(-0.764369010673889,1.,1.93147105496367));
#26244=CARTESIAN_POINT('Ctrl Pts',(-0.763954049121393,-1.,1.93768964875867));
#26245=CARTESIAN_POINT('Ctrl Pts',(-0.763954049121393,1.,1.93768964875867));
#26246=CARTESIAN_POINT('Ctrl Pts',(-0.76349533353858,-1.,1.94391746617626));
#26247=CARTESIAN_POINT('Ctrl Pts',(-0.76349533353858,1.,1.94391746617626));
#26248=CARTESIAN_POINT('Ctrl Pts',(-0.762992990878774,-1.,1.95015342590025));
#26249=CARTESIAN_POINT('Ctrl Pts',(-0.762992990878774,1.,1.95015342590025));
#26250=CARTESIAN_POINT('Ctrl Pts',(-0.762447203806263,-1.,1.95639665309893));
#26251=CARTESIAN_POINT('Ctrl Pts',(-0.762447203806263,1.,1.95639665309893));
#26252=CARTESIAN_POINT('Ctrl Pts',(-0.761858300014575,-1.,1.96264672744229));
#26253=CARTESIAN_POINT('Ctrl Pts',(-0.761858300014575,1.,1.96264672744229));
#26254=CARTESIAN_POINT('Ctrl Pts',(-0.761226690483986,-1.,1.96890351582545));
#26255=CARTESIAN_POINT('Ctrl Pts',(-0.761226690483986,1.,1.96890351582545));
#26256=CARTESIAN_POINT('Ctrl Pts',(-0.760552825409855,-1.,1.97516705321521));
#26257=CARTESIAN_POINT('Ctrl Pts',(-0.760552825409855,1.,1.97516705321521));
#26258=CARTESIAN_POINT('Ctrl Pts',(-0.759837147452135,-1.,1.98143741418156));
#26259=CARTESIAN_POINT('Ctrl Pts',(-0.759837147452135,1.,1.98143741418156));
#26260=CARTESIAN_POINT('Ctrl Pts',(-0.759080037802243,-1.,1.98771456680806));
#26261=CARTESIAN_POINT('Ctrl Pts',(-0.759080037802243,1.,1.98771456680806));
#26262=CARTESIAN_POINT('Ctrl Pts',(-0.758281796766377,-1.,1.9939983109871));
#26263=CARTESIAN_POINT('Ctrl Pts',(-0.758281796766377,1.,1.9939983109871));
#26264=CARTESIAN_POINT('Ctrl Pts',(-0.757442676862341,-1.,2.00028834739072));
#26265=CARTESIAN_POINT('Ctrl Pts',(-0.757442676862341,1.,2.00028834739072));
#26266=CARTESIAN_POINT('Ctrl Pts',(-0.756562904646496,-1.,2.00658431587682));
#26267=CARTESIAN_POINT('Ctrl Pts',(-0.756562904646496,1.,2.00658431587682));
#26268=CARTESIAN_POINT('Ctrl Pts',(-0.7556427049581,-1.,2.01288584328149));
#26269=CARTESIAN_POINT('Ctrl Pts',(-0.7556427049581,1.,2.01288584328149));
#26270=CARTESIAN_POINT('Ctrl Pts',(-0.75468233072352,-1.,2.01919259406003));
#26271=CARTESIAN_POINT('Ctrl Pts',(-0.75468233072352,1.,2.01919259406003));
#26272=CARTESIAN_POINT('Ctrl Pts',(-0.753682061113766,-1.,2.02550428623587));
#26273=CARTESIAN_POINT('Ctrl Pts',(-0.753682061113766,1.,2.02550428623587));
#26274=CARTESIAN_POINT('Ctrl Pts',(-0.752642180488104,-1.,2.03182068456467));
#26275=CARTESIAN_POINT('Ctrl Pts',(-0.752642180488104,1.,2.03182068456467));
#26276=CARTESIAN_POINT('Ctrl Pts',(-0.751562963361384,-1.,2.03814160092173));
#26277=CARTESIAN_POINT('Ctrl Pts',(-0.751562963361384,1.,2.03814160092173));
#26278=CARTESIAN_POINT('Ctrl Pts',(-0.750444657874758,-1.,2.04446689147754));
#26279=CARTESIAN_POINT('Ctrl Pts',(-0.750444657874758,1.,2.04446689147754));
#26280=CARTESIAN_POINT('Ctrl Pts',(-0.749287468663053,-1.,2.05079645591606));
#26281=CARTESIAN_POINT('Ctrl Pts',(-0.749287468663053,1.,2.05079645591606));
#26282=CARTESIAN_POINT('Ctrl Pts',(-0.748091554181101,-1.,2.05713023030263));
#26283=CARTESIAN_POINT('Ctrl Pts',(-0.748091554181101,1.,2.05713023030263));
#26284=CARTESIAN_POINT('Ctrl Pts',(-0.747103932785504,-1.,2.06220058927162));
#26285=CARTESIAN_POINT('Ctrl Pts',(-0.747103932785504,1.,2.06220058927162));
#26286=CARTESIAN_POINT('Ctrl Pts',(-0.746345871542696,-1.,2.06600523016401));
#26287=CARTESIAN_POINT('Ctrl Pts',(-0.746345871542696,1.,2.06600523016401));
#26288=CARTESIAN_POINT('Ctrl Pts',(-0.74583279137781,-1.,2.06854248895575));
#26289=CARTESIAN_POINT('Ctrl Pts',(-0.74583279137781,1.,2.06854248895575));
#26290=CARTESIAN_POINT('Ctrl Pts',(-0.745574324794401,-1.,2.0698113262342));
#26291=CARTESIAN_POINT('Ctrl Pts',(-0.745574324794401,1.,2.0698113262342));
#26292=CARTESIAN_POINT('',(-0.693717979106306,1.,1.60662857109684));
#26293=CARTESIAN_POINT('Ctrl Pts',(-0.693717979106306,1.,1.60662857109684));
#26294=CARTESIAN_POINT('Ctrl Pts',(-0.695712097881194,1.,1.61106790958151));
#26295=CARTESIAN_POINT('Ctrl Pts',(-0.699605146405088,1.,1.61974673472612));
#26296=CARTESIAN_POINT('Ctrl Pts',(-0.705159151988319,1.,1.63216541664676));
#26297=CARTESIAN_POINT('Ctrl Pts',(-0.711993139355394,1.,1.64752408832016));
#26298=CARTESIAN_POINT('Ctrl Pts',(-0.719585433804282,1.,1.6647288055568));
#26299=CARTESIAN_POINT('Ctrl Pts',(-0.726235967997433,1.,1.67996158455503));
#26300=CARTESIAN_POINT('Ctrl Pts',(-0.731963238697195,1.,1.69326921975743));
#26301=CARTESIAN_POINT('Ctrl Pts',(-0.736799665724771,1.,1.70473309006121));
#26302=CARTESIAN_POINT('Ctrl Pts',(-0.740795162032088,1.,1.71447789751927));
#26303=CARTESIAN_POINT('Ctrl Pts',(-0.744021445433764,1.,1.7226822991693));
#26304=CARTESIAN_POINT('Ctrl Pts',(-0.746574710096436,1.,1.72958533647399));
#26305=CARTESIAN_POINT('Ctrl Pts',(-0.748582462954855,1.,1.73550351679848));
#26306=CARTESIAN_POINT('Ctrl Pts',(-0.75019343597954,1.,1.74080458266705));
#26307=CARTESIAN_POINT('Ctrl Pts',(-0.751555614163629,1.,1.74585086852298));
#26308=CARTESIAN_POINT('Ctrl Pts',(-0.752797683531377,1.,1.75095139468809));
#26309=CARTESIAN_POINT('Ctrl Pts',(-0.75400925402848,1.,1.75631083600175));
#26310=CARTESIAN_POINT('Ctrl Pts',(-0.755220979975262,1.,1.7619781724032));
#26311=CARTESIAN_POINT('Ctrl Pts',(-0.756421896028403,1.,1.76789396003141));
#26312=CARTESIAN_POINT('Ctrl Pts',(-0.757578264077238,1.,1.77394167108342));
#26313=CARTESIAN_POINT('Ctrl Pts',(-0.75865062667738,1.,1.77999411220912));
#26314=CARTESIAN_POINT('Ctrl Pts',(-0.759614401109868,1.,1.78596964884526));
#26315=CARTESIAN_POINT('Ctrl Pts',(-0.760469555880425,1.,1.79185815610802));
#26316=CARTESIAN_POINT('Ctrl Pts',(-0.761229695230359,1.,1.79768986997735));
#26317=CARTESIAN_POINT('Ctrl Pts',(-0.761915336443516,1.,1.80351583877334));
#26318=CARTESIAN_POINT('Ctrl Pts',(-0.762546129464036,1.,1.80938551463989));
#26319=CARTESIAN_POINT('Ctrl Pts',(-0.763132003836783,1.,1.81532118405566));
#26320=CARTESIAN_POINT('Ctrl Pts',(-0.763673465462854,1.,1.82131873145297));
#26321=CARTESIAN_POINT('Ctrl Pts',(-0.764165902606055,1.,1.8273599120008));
#26322=CARTESIAN_POINT('Ctrl Pts',(-0.764602549687845,1.,1.8334207722714));
#26323=CARTESIAN_POINT('Ctrl Pts',(-0.764978057881687,1.,1.83948181064823));
#26324=CARTESIAN_POINT('Ctrl Pts',(-0.765291664861971,1.,1.8455369887591));
#26325=CARTESIAN_POINT('Ctrl Pts',(-0.765545710619023,1.,1.85158945130054));
#26326=CARTESIAN_POINT('Ctrl Pts',(-0.765744212909305,1.,1.85764741390391));
#26327=CARTESIAN_POINT('Ctrl Pts',(-0.765891519092557,1.,1.86372027063314));
#26328=CARTESIAN_POINT('Ctrl Pts',(-0.765990708546111,1.,1.86981398314345));
#26329=CARTESIAN_POINT('Ctrl Pts',(-0.766042837036759,1.,1.87592888967886));
#26330=CARTESIAN_POINT('Ctrl Pts',(-0.766047794851869,1.,1.88206215302561));
#26331=CARTESIAN_POINT('Ctrl Pts',(-0.76600483706209,1.,1.88820926433409));
#26332=CARTESIAN_POINT('Ctrl Pts',(-0.765913193856979,1.,1.89436577771389));
#26333=CARTESIAN_POINT('Ctrl Pts',(-0.765772772593395,1.,1.90052930393599));
#26334=CARTESIAN_POINT('Ctrl Pts',(-0.765584196937936,1.,1.90669961402362));
#26335=CARTESIAN_POINT('Ctrl Pts',(-0.765348465884739,1.,1.91287765805174));
#26336=CARTESIAN_POINT('Ctrl Pts',(-0.765066729667095,1.,1.91906491634197));
#26337=CARTESIAN_POINT('Ctrl Pts',(-0.764740025488189,1.,1.92526263537041));
#26338=CARTESIAN_POINT('Ctrl Pts',(-0.764369010673889,1.,1.93147105496367));
#26339=CARTESIAN_POINT('Ctrl Pts',(-0.763954049121393,1.,1.93768964875867));
#26340=CARTESIAN_POINT('Ctrl Pts',(-0.76349533353858,1.,1.94391746617626));
#26341=CARTESIAN_POINT('Ctrl Pts',(-0.762992990878774,1.,1.95015342590025));
#26342=CARTESIAN_POINT('Ctrl Pts',(-0.762447203806263,1.,1.95639665309893));
#26343=CARTESIAN_POINT('Ctrl Pts',(-0.761858300014575,1.,1.96264672744229));
#26344=CARTESIAN_POINT('Ctrl Pts',(-0.761226690483986,1.,1.96890351582545));
#26345=CARTESIAN_POINT('Ctrl Pts',(-0.760552825409855,1.,1.97516705321521));
#26346=CARTESIAN_POINT('Ctrl Pts',(-0.759837147452135,1.,1.98143741418156));
#26347=CARTESIAN_POINT('Ctrl Pts',(-0.759080037802243,1.,1.98771456680806));
#26348=CARTESIAN_POINT('Ctrl Pts',(-0.758281796766377,1.,1.9939983109871));
#26349=CARTESIAN_POINT('Ctrl Pts',(-0.757442676862341,1.,2.00028834739072));
#26350=CARTESIAN_POINT('Ctrl Pts',(-0.756562904646496,1.,2.00658431587682));
#26351=CARTESIAN_POINT('Ctrl Pts',(-0.7556427049581,1.,2.01288584328149));
#26352=CARTESIAN_POINT('Ctrl Pts',(-0.75468233072352,1.,2.01919259406003));
#26353=CARTESIAN_POINT('Ctrl Pts',(-0.753682061113766,1.,2.02550428623587));
#26354=CARTESIAN_POINT('Ctrl Pts',(-0.752642180488104,1.,2.03182068456467));
#26355=CARTESIAN_POINT('Ctrl Pts',(-0.751562963361384,1.,2.03814160092173));
#26356=CARTESIAN_POINT('Ctrl Pts',(-0.750444657874758,1.,2.04446689147754));
#26357=CARTESIAN_POINT('Ctrl Pts',(-0.749287468663053,1.,2.05079645591606));
#26358=CARTESIAN_POINT('Ctrl Pts',(-0.748091554181101,1.,2.05713023030263));
#26359=CARTESIAN_POINT('Ctrl Pts',(-0.747103932785504,1.,2.06220058927162));
#26360=CARTESIAN_POINT('Ctrl Pts',(-0.746345871542696,1.,2.06600523016401));
#26361=CARTESIAN_POINT('Ctrl Pts',(-0.74583279137781,1.,2.06854248895575));
#26362=CARTESIAN_POINT('Ctrl Pts',(-0.745574324794401,1.,2.0698113262342));
#26363=CARTESIAN_POINT('',(-0.693717979106306,0.,1.60662857109684));
#26364=CARTESIAN_POINT('Origin',(0.,0.,0.));
#26365=CARTESIAN_POINT('',(-0.892032620296855,1.,1.5055822144029));
#26366=CARTESIAN_POINT('Origin',(0.,1.,0.));
#26367=CARTESIAN_POINT('',(-0.892032620296855,0.,1.5055822144029));
#26368=CARTESIAN_POINT('Ctrl Pts',(-1.23627494547115,-1.,1.81978687191668));
#26369=CARTESIAN_POINT('Ctrl Pts',(-1.23627494547115,1.,1.81978687191668));
#26370=CARTESIAN_POINT('Ctrl Pts',(-1.23509651170476,-1.,1.81925017193666));
#26371=CARTESIAN_POINT('Ctrl Pts',(-1.23509651170476,1.,1.81925017193666));
#26372=CARTESIAN_POINT('Ctrl Pts',(-1.2327422452705,-1.,1.81817389921279));
#26373=CARTESIAN_POINT('Ctrl Pts',(-1.2327422452705,1.,1.81817389921279));
#26374=CARTESIAN_POINT('Ctrl Pts',(-1.2292186489137,-1.,1.8165508718364));
#26375=CARTESIAN_POINT('Ctrl Pts',(-1.2292186489137,1.,1.8165508718364));
#26376=CARTESIAN_POINT('Ctrl Pts',(-1.2245361330495,-1.,1.81436959210434));
#26377=CARTESIAN_POINT('Ctrl Pts',(-1.2245361330495,1.,1.81436959210434));
#26378=CARTESIAN_POINT('Ctrl Pts',(-1.21870906103557,-1.,1.81161420806656));
#26379=CARTESIAN_POINT('Ctrl Pts',(-1.21870906103557,1.,1.81161420806656));
#26380=CARTESIAN_POINT('Ctrl Pts',(-1.21290815708314,-1.,1.80882996917129));
#26381=CARTESIAN_POINT('Ctrl Pts',(-1.21290815708314,1.,1.80882996917129));
#26382=CARTESIAN_POINT('Ctrl Pts',(-1.20713356605475,-1.,1.80601678480707));
#26383=CARTESIAN_POINT('Ctrl Pts',(-1.20713356605475,1.,1.80601678480707));
#26384=CARTESIAN_POINT('Ctrl Pts',(-1.20138548938974,-1.,1.80317454838603));
#26385=CARTESIAN_POINT('Ctrl Pts',(-1.20138548938974,1.,1.80317454838603));
#26386=CARTESIAN_POINT('Ctrl Pts',(-1.19566418930242,-1.,1.80030314369879));
#26387=CARTESIAN_POINT('Ctrl Pts',(-1.19566418930242,1.,1.80030314369879));
#26388=CARTESIAN_POINT('Ctrl Pts',(-1.18996997934445,-1.,1.79740245923478));
#26389=CARTESIAN_POINT('Ctrl Pts',(-1.18996997934445,1.,1.79740245923478));
#26390=CARTESIAN_POINT('Ctrl Pts',(-1.18430321697432,-1.,1.79447240321515));
#26391=CARTESIAN_POINT('Ctrl Pts',(-1.18430321697432,1.,1.79447240321515));
#26392=CARTESIAN_POINT('Ctrl Pts',(-1.17866429440809,-1.,1.79151291552689));
#26393=CARTESIAN_POINT('Ctrl Pts',(-1.17866429440809,1.,1.79151291552689));
#26394=CARTESIAN_POINT('Ctrl Pts',(-1.17305363177328,-1.,1.78852398877616));
#26395=CARTESIAN_POINT('Ctrl Pts',(-1.17305363177328,1.,1.78852398877616));
#26396=CARTESIAN_POINT('Ctrl Pts',(-1.16747166312303,-1.,1.78550566040443));
#26397=CARTESIAN_POINT('Ctrl Pts',(-1.16747166312303,1.,1.78550566040443));
#26398=CARTESIAN_POINT('Ctrl Pts',(-1.16191881298499,-1.,1.78245795881009));
#26399=CARTESIAN_POINT('Ctrl Pts',(-1.16191881298499,1.,1.78245795881009));
#26400=CARTESIAN_POINT('Ctrl Pts',(-1.15639547194698,-1.,1.77938085564275));
#26401=CARTESIAN_POINT('Ctrl Pts',(-1.15639547194698,1.,1.77938085564275));
#26402=CARTESIAN_POINT('Ctrl Pts',(-1.15090197841515,-1.,1.7762742255701));
#26403=CARTESIAN_POINT('Ctrl Pts',(-1.15090197841515,1.,1.7762742255701));
#26404=CARTESIAN_POINT('Ctrl Pts',(-1.1454385822692,-1.,1.77313777896194));
#26405=CARTESIAN_POINT('Ctrl Pts',(-1.1454385822692,1.,1.77313777896194));
#26406=CARTESIAN_POINT('Ctrl Pts',(-1.14000548336975,-1.,1.76997111386769));
#26407=CARTESIAN_POINT('Ctrl Pts',(-1.14000548336975,1.,1.76997111386769));
#26408=CARTESIAN_POINT('Ctrl Pts',(-1.1346029180462,-1.,1.76677384551862));
#26409=CARTESIAN_POINT('Ctrl Pts',(-1.1346029180462,1.,1.76677384551862));
#26410=CARTESIAN_POINT('Ctrl Pts',(-1.12923123555075,-1.,1.7635457196617));
#26411=CARTESIAN_POINT('Ctrl Pts',(-1.12923123555075,1.,1.7635457196617));
#26412=CARTESIAN_POINT('Ctrl Pts',(-1.12389096855086,-1.,1.76028671825096));
#26413=CARTESIAN_POINT('Ctrl Pts',(-1.12389096855086,1.,1.76028671825096));
#26414=CARTESIAN_POINT('Ctrl Pts',(-1.11858293216763,-1.,1.75699720772105));
#26415=CARTESIAN_POINT('Ctrl Pts',(-1.11858293216763,1.,1.75699720772105));
#26416=CARTESIAN_POINT('Ctrl Pts',(-1.11330807582551,-1.,1.7536777209463));
#26417=CARTESIAN_POINT('Ctrl Pts',(-1.11330807582551,1.,1.7536777209463));
#26418=CARTESIAN_POINT('Ctrl Pts',(-1.10806728183007,-1.,1.7503286607592));
#26419=CARTESIAN_POINT('Ctrl Pts',(-1.10806728183007,1.,1.7503286607592));
#26420=CARTESIAN_POINT('Ctrl Pts',(-1.10286118991143,-1.,1.74695004214923));
#26421=CARTESIAN_POINT('Ctrl Pts',(-1.10286118991143,1.,1.74695004214923));
#26422=CARTESIAN_POINT('Ctrl Pts',(-1.09768999241225,-1.,1.74354119236208));
#26423=CARTESIAN_POINT('Ctrl Pts',(-1.09768999241225,1.,1.74354119236208));
#26424=CARTESIAN_POINT('Ctrl Pts',(-1.09255329056493,-1.,1.74010053962247));
#26425=CARTESIAN_POINT('Ctrl Pts',(-1.09255329056493,1.,1.74010053962247));
#26426=CARTESIAN_POINT('Ctrl Pts',(-1.08745056285427,-1.,1.73662628326091));
#26427=CARTESIAN_POINT('Ctrl Pts',(-1.08745056285427,1.,1.73662628326091));
#26428=CARTESIAN_POINT('Ctrl Pts',(-1.08238162784749,-1.,1.73311705663407));
#26429=CARTESIAN_POINT('Ctrl Pts',(-1.08238162784749,1.,1.73311705663407));
#26430=CARTESIAN_POINT('Ctrl Pts',(-1.0773470373727,-1.,1.72957248977424));
#26431=CARTESIAN_POINT('Ctrl Pts',(-1.0773470373727,1.,1.72957248977424));
#26432=CARTESIAN_POINT('Ctrl Pts',(-1.07234866990252,-1.,1.72599406198488));
#26433=CARTESIAN_POINT('Ctrl Pts',(-1.07234866990252,1.,1.72599406198488));
#26434=CARTESIAN_POINT('Ctrl Pts',(-1.06738966975462,-1.,1.72238500928453));
#26435=CARTESIAN_POINT('Ctrl Pts',(-1.06738966975462,1.,1.72238500928453));
#26436=CARTESIAN_POINT('Ctrl Pts',(-1.06247324680647,-1.,1.71874858456904));
#26437=CARTESIAN_POINT('Ctrl Pts',(-1.06247324680647,1.,1.71874858456904));
#26438=CARTESIAN_POINT('Ctrl Pts',(-1.05760163192479,-1.,1.7150865442702));
#26439=CARTESIAN_POINT('Ctrl Pts',(-1.05760163192479,1.,1.7150865442702));
#26440=CARTESIAN_POINT('Ctrl Pts',(-1.05277517202855,-1.,1.71139783543989));
#26441=CARTESIAN_POINT('Ctrl Pts',(-1.05277517202855,1.,1.71139783543989));
#26442=CARTESIAN_POINT('Ctrl Pts',(-1.04799085404995,-1.,1.70767646263649));
#26443=CARTESIAN_POINT('Ctrl Pts',(-1.04799085404995,1.,1.70767646263649));
#26444=CARTESIAN_POINT('Ctrl Pts',(-1.04324363334554,-1.,1.70391338707982));
#26445=CARTESIAN_POINT('Ctrl Pts',(-1.04324363334554,1.,1.70391338707982));
#26446=CARTESIAN_POINT('Ctrl Pts',(-1.03852922490789,-1.,1.70010052930962));
#26447=CARTESIAN_POINT('Ctrl Pts',(-1.03852922490789,1.,1.70010052930962));
#26448=CARTESIAN_POINT('Ctrl Pts',(-1.03384646003588,-1.,1.69623414782771));
#26449=CARTESIAN_POINT('Ctrl Pts',(-1.03384646003588,1.,1.69623414782771));
#26450=CARTESIAN_POINT('Ctrl Pts',(-1.02919977579147,-1.,1.69231840863458));
#26451=CARTESIAN_POINT('Ctrl Pts',(-1.02919977579147,1.,1.69231840863458));
#26452=CARTESIAN_POINT('Ctrl Pts',(-1.02460180535255,-1.,1.68836910178447));
#26453=CARTESIAN_POINT('Ctrl Pts',(-1.02460180535255,1.,1.68836910178447));
#26454=CARTESIAN_POINT('Ctrl Pts',(-1.02006795074201,-1.,1.68440578021706));
#26455=CARTESIAN_POINT('Ctrl Pts',(-1.02006795074201,1.,1.68440578021706));
#26456=CARTESIAN_POINT('Ctrl Pts',(-1.01561026162773,-1.,1.68044289894798));
#26457=CARTESIAN_POINT('Ctrl Pts',(-1.01561026162773,1.,1.68044289894798));
#26458=CARTESIAN_POINT('Ctrl Pts',(-1.01123236493511,-1.,1.67648246776464));
#26459=CARTESIAN_POINT('Ctrl Pts',(-1.01123236493511,1.,1.67648246776464));
#26460=CARTESIAN_POINT('Ctrl Pts',(-1.00692206696414,-1.,1.67250335383293));
#26461=CARTESIAN_POINT('Ctrl Pts',(-1.00692206696414,1.,1.67250335383293));
#26462=CARTESIAN_POINT('Ctrl Pts',(-1.00265091003727,-1.,1.66846059277303));
#26463=CARTESIAN_POINT('Ctrl Pts',(-1.00265091003727,1.,1.66846059277303));
#26464=CARTESIAN_POINT('Ctrl Pts',(-0.998389654952758,-1.,1.66430758030376));
#26465=CARTESIAN_POINT('Ctrl Pts',(-0.998389654952758,1.,1.66430758030376));
#26466=CARTESIAN_POINT('Ctrl Pts',(-0.994121836661306,-1.,1.66001553809947));
#26467=CARTESIAN_POINT('Ctrl Pts',(-0.994121836661306,1.,1.66001553809947));
#26468=CARTESIAN_POINT('Ctrl Pts',(-0.989855627854165,-1.,1.65559044289699));
#26469=CARTESIAN_POINT('Ctrl Pts',(-0.989855627854165,1.,1.65559044289699));
#26470=CARTESIAN_POINT('Ctrl Pts',(-0.985642622920821,-1.,1.65110016612638));
#26471=CARTESIAN_POINT('Ctrl Pts',(-0.985642622920821,1.,1.65110016612638));
#26472=CARTESIAN_POINT('Ctrl Pts',(-0.981562530939489,-1.,1.64665139190656));
#26473=CARTESIAN_POINT('Ctrl Pts',(-0.981562530939489,1.,1.64665139190656));
#26474=CARTESIAN_POINT('Ctrl Pts',(-0.977689794119416,-1.,1.64233990826687));
#26475=CARTESIAN_POINT('Ctrl Pts',(-0.977689794119416,1.,1.64233990826687));
#26476=CARTESIAN_POINT('Ctrl Pts',(-0.974066058287418,-1.,1.63820952658144));
#26477=CARTESIAN_POINT('Ctrl Pts',(-0.974066058287418,1.,1.63820952658144));
#26478=CARTESIAN_POINT('Ctrl Pts',(-0.970669715997509,-1.,1.63420665729798));
#26479=CARTESIAN_POINT('Ctrl Pts',(-0.970669715997509,1.,1.63420665729798));
#26480=CARTESIAN_POINT('Ctrl Pts',(-0.967387853230345,-1.,1.63013849959461));
#26481=CARTESIAN_POINT('Ctrl Pts',(-0.967387853230345,1.,1.63013849959461));
#26482=CARTESIAN_POINT('Ctrl Pts',(-0.964046107040536,-1.,1.62571930670187));
#26483=CARTESIAN_POINT('Ctrl Pts',(-0.964046107040536,1.,1.62571930670187));
#26484=CARTESIAN_POINT('Ctrl Pts',(-0.960438326101729,-1.,1.62061638140221));
#26485=CARTESIAN_POINT('Ctrl Pts',(-0.960438326101729,1.,1.62061638140221));
#26486=CARTESIAN_POINT('Ctrl Pts',(-0.956354422920671,-1.,1.61449324337085));
#26487=CARTESIAN_POINT('Ctrl Pts',(-0.956354422920671,1.,1.61449324337085));
#26488=CARTESIAN_POINT('Ctrl Pts',(-0.951613284356035,-1.,1.60706069896936));
#26489=CARTESIAN_POINT('Ctrl Pts',(-0.951613284356035,1.,1.60706069896936));
#26490=CARTESIAN_POINT('Ctrl Pts',(-0.946078063315257,-1.,1.59810042043673));
#26491=CARTESIAN_POINT('Ctrl Pts',(-0.946078063315257,1.,1.59810042043673));
#26492=CARTESIAN_POINT('Ctrl Pts',(-0.939646377893399,-1.,1.58744937487176));
#26493=CARTESIAN_POINT('Ctrl Pts',(-0.939646377893399,1.,1.58744937487176));
#26494=CARTESIAN_POINT('Ctrl Pts',(-0.932246680108685,-1.,1.57499388382243));
#26495=CARTESIAN_POINT('Ctrl Pts',(-0.932246680108685,1.,1.57499388382243));
#26496=CARTESIAN_POINT('Ctrl Pts',(-0.923832188944341,-1.,1.56065988578893));
#26497=CARTESIAN_POINT('Ctrl Pts',(-0.923832188944341,1.,1.56065988578893));
#26498=CARTESIAN_POINT('Ctrl Pts',(-0.914375919026456,-1.,1.54440491149498));
#26499=CARTESIAN_POINT('Ctrl Pts',(-0.914375919026456,1.,1.54440491149498));
#26500=CARTESIAN_POINT('Ctrl Pts',(-0.905967409625651,-1.,1.52984849887993));
#26501=CARTESIAN_POINT('Ctrl Pts',(-0.905967409625651,1.,1.52984849887993));
#26502=CARTESIAN_POINT('Ctrl Pts',(-0.899185047483511,-1.,1.51805569590094));
#26503=CARTESIAN_POINT('Ctrl Pts',(-0.899185047483511,1.,1.51805569590094));
#26504=CARTESIAN_POINT('Ctrl Pts',(-0.894452006964543,-1.,1.50980486806688));
#26505=CARTESIAN_POINT('Ctrl Pts',(-0.894452006964543,1.,1.50980486806688));
#26506=CARTESIAN_POINT('Ctrl Pts',(-0.892032620296855,-1.,1.5055822144029));
#26507=CARTESIAN_POINT('Ctrl Pts',(-0.892032620296855,1.,1.5055822144029));
#26508=CARTESIAN_POINT('',(-1.23627494547115,1.,1.81978687191668));
#26509=CARTESIAN_POINT('Ctrl Pts',(-1.23627494547115,1.,1.81978687191668));
#26510=CARTESIAN_POINT('Ctrl Pts',(-1.23509651170476,1.,1.81925017193666));
#26511=CARTESIAN_POINT('Ctrl Pts',(-1.2327422452705,1.,1.81817389921279));
#26512=CARTESIAN_POINT('Ctrl Pts',(-1.2292186489137,1.,1.8165508718364));
#26513=CARTESIAN_POINT('Ctrl Pts',(-1.2245361330495,1.,1.81436959210434));
#26514=CARTESIAN_POINT('Ctrl Pts',(-1.21870906103557,1.,1.81161420806656));
#26515=CARTESIAN_POINT('Ctrl Pts',(-1.21290815708314,1.,1.80882996917129));
#26516=CARTESIAN_POINT('Ctrl Pts',(-1.20713356605475,1.,1.80601678480707));
#26517=CARTESIAN_POINT('Ctrl Pts',(-1.20138548938974,1.,1.80317454838603));
#26518=CARTESIAN_POINT('Ctrl Pts',(-1.19566418930242,1.,1.80030314369879));
#26519=CARTESIAN_POINT('Ctrl Pts',(-1.18996997934445,1.,1.79740245923478));
#26520=CARTESIAN_POINT('Ctrl Pts',(-1.18430321697432,1.,1.79447240321515));
#26521=CARTESIAN_POINT('Ctrl Pts',(-1.17866429440809,1.,1.79151291552689));
#26522=CARTESIAN_POINT('Ctrl Pts',(-1.17305363177328,1.,1.78852398877616));
#26523=CARTESIAN_POINT('Ctrl Pts',(-1.16747166312303,1.,1.78550566040443));
#26524=CARTESIAN_POINT('Ctrl Pts',(-1.16191881298499,1.,1.78245795881009));
#26525=CARTESIAN_POINT('Ctrl Pts',(-1.15639547194698,1.,1.77938085564275));
#26526=CARTESIAN_POINT('Ctrl Pts',(-1.15090197841515,1.,1.7762742255701));
#26527=CARTESIAN_POINT('Ctrl Pts',(-1.1454385822692,1.,1.77313777896194));
#26528=CARTESIAN_POINT('Ctrl Pts',(-1.14000548336975,1.,1.76997111386769));
#26529=CARTESIAN_POINT('Ctrl Pts',(-1.1346029180462,1.,1.76677384551862));
#26530=CARTESIAN_POINT('Ctrl Pts',(-1.12923123555075,1.,1.7635457196617));
#26531=CARTESIAN_POINT('Ctrl Pts',(-1.12389096855086,1.,1.76028671825096));
#26532=CARTESIAN_POINT('Ctrl Pts',(-1.11858293216763,1.,1.75699720772105));
#26533=CARTESIAN_POINT('Ctrl Pts',(-1.11330807582551,1.,1.7536777209463));
#26534=CARTESIAN_POINT('Ctrl Pts',(-1.10806728183007,1.,1.7503286607592));
#26535=CARTESIAN_POINT('Ctrl Pts',(-1.10286118991143,1.,1.74695004214923));
#26536=CARTESIAN_POINT('Ctrl Pts',(-1.09768999241225,1.,1.74354119236208));
#26537=CARTESIAN_POINT('Ctrl Pts',(-1.09255329056493,1.,1.74010053962247));
#26538=CARTESIAN_POINT('Ctrl Pts',(-1.08745056285427,1.,1.73662628326091));
#26539=CARTESIAN_POINT('Ctrl Pts',(-1.08238162784749,1.,1.73311705663407));
#26540=CARTESIAN_POINT('Ctrl Pts',(-1.0773470373727,1.,1.72957248977424));
#26541=CARTESIAN_POINT('Ctrl Pts',(-1.07234866990252,1.,1.72599406198488));
#26542=CARTESIAN_POINT('Ctrl Pts',(-1.06738966975462,1.,1.72238500928453));
#26543=CARTESIAN_POINT('Ctrl Pts',(-1.06247324680647,1.,1.71874858456904));
#26544=CARTESIAN_POINT('Ctrl Pts',(-1.05760163192479,1.,1.7150865442702));
#26545=CARTESIAN_POINT('Ctrl Pts',(-1.05277517202855,1.,1.71139783543989));
#26546=CARTESIAN_POINT('Ctrl Pts',(-1.04799085404995,1.,1.70767646263649));
#26547=CARTESIAN_POINT('Ctrl Pts',(-1.04324363334554,1.,1.70391338707982));
#26548=CARTESIAN_POINT('Ctrl Pts',(-1.03852922490789,1.,1.70010052930962));
#26549=CARTESIAN_POINT('Ctrl Pts',(-1.03384646003588,1.,1.69623414782771));
#26550=CARTESIAN_POINT('Ctrl Pts',(-1.02919977579147,1.,1.69231840863458));
#26551=CARTESIAN_POINT('Ctrl Pts',(-1.02460180535255,1.,1.68836910178447));
#26552=CARTESIAN_POINT('Ctrl Pts',(-1.02006795074201,1.,1.68440578021706));
#26553=CARTESIAN_POINT('Ctrl Pts',(-1.01561026162773,1.,1.68044289894798));
#26554=CARTESIAN_POINT('Ctrl Pts',(-1.01123236493511,1.,1.67648246776464));
#26555=CARTESIAN_POINT('Ctrl Pts',(-1.00692206696414,1.,1.67250335383293));
#26556=CARTESIAN_POINT('Ctrl Pts',(-1.00265091003727,1.,1.66846059277303));
#26557=CARTESIAN_POINT('Ctrl Pts',(-0.998389654952758,1.,1.66430758030376));
#26558=CARTESIAN_POINT('Ctrl Pts',(-0.994121836661306,1.,1.66001553809947));
#26559=CARTESIAN_POINT('Ctrl Pts',(-0.989855627854165,1.,1.65559044289699));
#26560=CARTESIAN_POINT('Ctrl Pts',(-0.985642622920821,1.,1.65110016612638));
#26561=CARTESIAN_POINT('Ctrl Pts',(-0.981562530939489,1.,1.64665139190656));
#26562=CARTESIAN_POINT('Ctrl Pts',(-0.977689794119416,1.,1.64233990826687));
#26563=CARTESIAN_POINT('Ctrl Pts',(-0.974066058287418,1.,1.63820952658144));
#26564=CARTESIAN_POINT('Ctrl Pts',(-0.970669715997509,1.,1.63420665729798));
#26565=CARTESIAN_POINT('Ctrl Pts',(-0.967387853230345,1.,1.63013849959461));
#26566=CARTESIAN_POINT('Ctrl Pts',(-0.964046107040536,1.,1.62571930670187));
#26567=CARTESIAN_POINT('Ctrl Pts',(-0.960438326101729,1.,1.62061638140221));
#26568=CARTESIAN_POINT('Ctrl Pts',(-0.956354422920671,1.,1.61449324337085));
#26569=CARTESIAN_POINT('Ctrl Pts',(-0.951613284356035,1.,1.60706069896936));
#26570=CARTESIAN_POINT('Ctrl Pts',(-0.946078063315257,1.,1.59810042043673));
#26571=CARTESIAN_POINT('Ctrl Pts',(-0.939646377893399,1.,1.58744937487176));
#26572=CARTESIAN_POINT('Ctrl Pts',(-0.932246680108685,1.,1.57499388382243));
#26573=CARTESIAN_POINT('Ctrl Pts',(-0.923832188944341,1.,1.56065988578893));
#26574=CARTESIAN_POINT('Ctrl Pts',(-0.914375919026456,1.,1.54440491149498));
#26575=CARTESIAN_POINT('Ctrl Pts',(-0.905967409625651,1.,1.52984849887993));
#26576=CARTESIAN_POINT('Ctrl Pts',(-0.899185047483511,1.,1.51805569590094));
#26577=CARTESIAN_POINT('Ctrl Pts',(-0.894452006964543,1.,1.50980486806688));
#26578=CARTESIAN_POINT('Ctrl Pts',(-0.892032620296855,1.,1.5055822144029));
#26579=CARTESIAN_POINT('',(-1.23627494547115,0.,1.81978687191668));
#26580=CARTESIAN_POINT('Origin',(-1.34869019493419,0.,1.73811241238545));
#26581=CARTESIAN_POINT('',(-1.34869019493419,1.,1.73811241238545));
#26582=CARTESIAN_POINT('',(-1.23627494547115,1.,1.81978687191668));
#26583=CARTESIAN_POINT('',(-1.34869019493419,0.,1.73811241238545));
#26584=CARTESIAN_POINT('Ctrl Pts',(-1.15624053661742,-1.,1.31362392696032));
#26585=CARTESIAN_POINT('Ctrl Pts',(-1.15624053661742,1.,1.31362392696032));
#26586=CARTESIAN_POINT('Ctrl Pts',(-1.15950888730809,-1.,1.31722977216397));
#26587=CARTESIAN_POINT('Ctrl Pts',(-1.15950888730809,1.,1.31722977216397));
#26588=CARTESIAN_POINT('Ctrl Pts',(-1.16589330093588,-1.,1.32428080721772));
#26589=CARTESIAN_POINT('Ctrl Pts',(-1.16589330093588,1.,1.32428080721772));
#26590=CARTESIAN_POINT('Ctrl Pts',(-1.17501305789857,-1.,1.33437539347008));
#26591=CARTESIAN_POINT('Ctrl Pts',(-1.17501305789857,1.,1.33437539347008));
#26592=CARTESIAN_POINT('Ctrl Pts',(-1.18625865667441,-1.,1.34687054001093));
#26593=CARTESIAN_POINT('Ctrl Pts',(-1.18625865667441,1.,1.34687054001093));
#26594=CARTESIAN_POINT('Ctrl Pts',(-1.1987959077932,-1.,1.36088705043885));
#26595=CARTESIAN_POINT('Ctrl Pts',(-1.1987959077932,1.,1.36088705043885));
#26596=CARTESIAN_POINT('Ctrl Pts',(-1.20982812925645,-1.,1.37331915607905));
#26597=CARTESIAN_POINT('Ctrl Pts',(-1.20982812925645,1.,1.37331915607905));
#26598=CARTESIAN_POINT('Ctrl Pts',(-1.21938737280852,-1.,1.38420564527715));
#26599=CARTESIAN_POINT('Ctrl Pts',(-1.21938737280852,1.,1.38420564527715));
#26600=CARTESIAN_POINT('Ctrl Pts',(-1.22752961899387,-1.,1.39361389568796));
#26601=CARTESIAN_POINT('Ctrl Pts',(-1.22752961899387,1.,1.39361389568796));
#26602=CARTESIAN_POINT('Ctrl Pts',(-1.23434087290423,-1.,1.40164708206106));
#26603=CARTESIAN_POINT('Ctrl Pts',(-1.23434087290423,1.,1.40164708206106));
#26604=CARTESIAN_POINT('Ctrl Pts',(-1.23994455029534,-1.,1.40845295531283));
#26605=CARTESIAN_POINT('Ctrl Pts',(-1.23994455029534,1.,1.40845295531283));
#26606=CARTESIAN_POINT('Ctrl Pts',(-1.24450600513056,-1.,1.41422913175179));
#26607=CARTESIAN_POINT('Ctrl Pts',(-1.24450600513056,1.,1.41422913175179));
#26608=CARTESIAN_POINT('Ctrl Pts',(-1.24824430986571,-1.,1.41923722596025));
#26609=CARTESIAN_POINT('Ctrl Pts',(-1.24824430986571,1.,1.41923722596025));
#26610=CARTESIAN_POINT('Ctrl Pts',(-1.2514145557001,-1.,1.42378102115575));
#26611=CARTESIAN_POINT('Ctrl Pts',(-1.2514145557001,1.,1.42378102115575));
#26612=CARTESIAN_POINT('Ctrl Pts',(-1.25426945222639,-1.,1.42815938799387));
#26613=CARTESIAN_POINT('Ctrl Pts',(-1.25426945222639,1.,1.42815938799387));
#26614=CARTESIAN_POINT('Ctrl Pts',(-1.25702687965755,-1.,1.43262645609691));
#26615=CARTESIAN_POINT('Ctrl Pts',(-1.25702687965755,1.,1.43262645609691));
#26616=CARTESIAN_POINT('Ctrl Pts',(-1.25983531012005,-1.,1.43734919180848));
#26617=CARTESIAN_POINT('Ctrl Pts',(-1.25983531012005,1.,1.43734919180848));
#26618=CARTESIAN_POINT('Ctrl Pts',(-1.26273903323859,-1.,1.44236470511303));
#26619=CARTESIAN_POINT('Ctrl Pts',(-1.26273903323859,1.,1.44236470511303));
#26620=CARTESIAN_POINT('Ctrl Pts',(-1.26570925118868,-1.,1.44761985001662));
#26621=CARTESIAN_POINT('Ctrl Pts',(-1.26570925118868,1.,1.44761985001662));
#26622=CARTESIAN_POINT('Ctrl Pts',(-1.2686778680489,-1.,1.45301422764247));
#26623=CARTESIAN_POINT('Ctrl Pts',(-1.2686778680489,1.,1.45301422764247));
#26624=CARTESIAN_POINT('Ctrl Pts',(-1.27156805265289,-1.,1.45843906294697));
#26625=CARTESIAN_POINT('Ctrl Pts',(-1.27156805265289,1.,1.45843906294697));
#26626=CARTESIAN_POINT('Ctrl Pts',(-1.27433119897822,-1.,1.46382431332476));
#26627=CARTESIAN_POINT('Ctrl Pts',(-1.27433119897822,1.,1.46382431332476));
#26628=CARTESIAN_POINT('Ctrl Pts',(-1.27696414831089,-1.,1.46916035917133));
#26629=CARTESIAN_POINT('Ctrl Pts',(-1.27696414831089,1.,1.46916035917133));
#26630=CARTESIAN_POINT('Ctrl Pts',(-1.2794891824849,-1.,1.4744717526707));
#26631=CARTESIAN_POINT('Ctrl Pts',(-1.2794891824849,1.,1.4744717526707));
#26632=CARTESIAN_POINT('Ctrl Pts',(-1.28194158939517,-1.,1.47980070347095));
#26633=CARTESIAN_POINT('Ctrl Pts',(-1.28194158939517,1.,1.47980070347095));
#26634=CARTESIAN_POINT('Ctrl Pts',(-1.28435533880201,-1.,1.4851881711891));
#26635=CARTESIAN_POINT('Ctrl Pts',(-1.28435533880201,1.,1.4851881711891));
#26636=CARTESIAN_POINT('Ctrl Pts',(-1.2867467611644,-1.,1.4906522831278));
#26637=CARTESIAN_POINT('Ctrl Pts',(-1.2867467611644,1.,1.4906522831278));
#26638=CARTESIAN_POINT('Ctrl Pts',(-1.28911506584254,-1.,1.49618896881754));
#26639=CARTESIAN_POINT('Ctrl Pts',(-1.28911506584254,1.,1.49618896881754));
#26640=CARTESIAN_POINT('Ctrl Pts',(-1.29145022885181,-1.,1.50178230149776));
#26641=CARTESIAN_POINT('Ctrl Pts',(-1.29145022885181,1.,1.50178230149776));
#26642=CARTESIAN_POINT('Ctrl Pts',(-1.29373841372842,-1.,1.50741159078365));
#26643=CARTESIAN_POINT('Ctrl Pts',(-1.29373841372842,1.,1.50741159078365));
#26644=CARTESIAN_POINT('Ctrl Pts',(-1.29596850710509,-1.,1.51305994241402));
#26645=CARTESIAN_POINT('Ctrl Pts',(-1.29596850710509,1.,1.51305994241402));
#26646=CARTESIAN_POINT('Ctrl Pts',(-1.29813791800747,-1.,1.51872184912724));
#26647=CARTESIAN_POINT('Ctrl Pts',(-1.29813791800747,1.,1.51872184912724));
#26648=CARTESIAN_POINT('Ctrl Pts',(-1.30024984366328,-1.,1.52439957861062));
#26649=CARTESIAN_POINT('Ctrl Pts',(-1.30024984366328,1.,1.52439957861062));
#26650=CARTESIAN_POINT('Ctrl Pts',(-1.30231064395568,-1.,1.53009970283891));
#26651=CARTESIAN_POINT('Ctrl Pts',(-1.30231064395568,1.,1.53009970283891));
#26652=CARTESIAN_POINT('Ctrl Pts',(-1.30432735639489,-1.,1.53582981268977));
#26653=CARTESIAN_POINT('Ctrl Pts',(-1.30432735639489,1.,1.53582981268977));
#26654=CARTESIAN_POINT('Ctrl Pts',(-1.30630475189556,-1.,1.54159462645432));
#26655=CARTESIAN_POINT('Ctrl Pts',(-1.30630475189556,1.,1.54159462645432));
#26656=CARTESIAN_POINT('Ctrl Pts',(-1.30824393907473,-1.,1.54739413957185));
#26657=CARTESIAN_POINT('Ctrl Pts',(-1.30824393907473,1.,1.54739413957185));
#26658=CARTESIAN_POINT('Ctrl Pts',(-1.31014393684222,-1.,1.55322568759481));
#26659=CARTESIAN_POINT('Ctrl Pts',(-1.31014393684222,1.,1.55322568759481));
#26660=CARTESIAN_POINT('Ctrl Pts',(-1.31200264341696,-1.,1.55908521254821));
#26661=CARTESIAN_POINT('Ctrl Pts',(-1.31200264341696,1.,1.55908521254821));
#26662=CARTESIAN_POINT('Ctrl Pts',(-1.31381795281002,-1.,1.56496872402353));
#26663=CARTESIAN_POINT('Ctrl Pts',(-1.31381795281002,1.,1.56496872402353));
#26664=CARTESIAN_POINT('Ctrl Pts',(-1.31558903860016,-1.,1.57087397835723));
#26665=CARTESIAN_POINT('Ctrl Pts',(-1.31558903860016,1.,1.57087397835723));
#26666=CARTESIAN_POINT('Ctrl Pts',(-1.31731642317187,-1.,1.5768005650559));
#26667=CARTESIAN_POINT('Ctrl Pts',(-1.31731642317187,1.,1.5768005650559));
#26668=CARTESIAN_POINT('Ctrl Pts',(-1.31900135021432,-1.,1.58274907898834));
#26669=CARTESIAN_POINT('Ctrl Pts',(-1.31900135021432,1.,1.58274907898834));
#26670=CARTESIAN_POINT('Ctrl Pts',(-1.32064537110892,-1.,1.58872057258245));
#26671=CARTESIAN_POINT('Ctrl Pts',(-1.32064537110892,1.,1.58872057258245));
#26672=CARTESIAN_POINT('Ctrl Pts',(-1.32224985747682,-1.,1.59471591079403));
#26673=CARTESIAN_POINT('Ctrl Pts',(-1.32224985747682,1.,1.59471591079403));
#26674=CARTESIAN_POINT('Ctrl Pts',(-1.32381550858256,-1.,1.60073511858687));
#26675=CARTESIAN_POINT('Ctrl Pts',(-1.32381550858256,1.,1.60073511858687));
#26676=CARTESIAN_POINT('Ctrl Pts',(-1.32534250785782,-1.,1.60677758290954));
#26677=CARTESIAN_POINT('Ctrl Pts',(-1.32534250785782,1.,1.60677758290954));
#26678=CARTESIAN_POINT('Ctrl Pts',(-1.32683074483356,-1.,1.6128423401575));
#26679=CARTESIAN_POINT('Ctrl Pts',(-1.32683074483356,1.,1.6128423401575));
#26680=CARTESIAN_POINT('Ctrl Pts',(-1.32828000610449,-1.,1.61892832270724));
#26681=CARTESIAN_POINT('Ctrl Pts',(-1.32828000610449,1.,1.61892832270724));
#26682=CARTESIAN_POINT('Ctrl Pts',(-1.3296901950568,-1.,1.62503464209797));
#26683=CARTESIAN_POINT('Ctrl Pts',(-1.3296901950568,1.,1.62503464209797));
#26684=CARTESIAN_POINT('Ctrl Pts',(-1.33106149345645,-1.,1.63116079730923));
#26685=CARTESIAN_POINT('Ctrl Pts',(-1.33106149345645,1.,1.63116079730923));
#26686=CARTESIAN_POINT('Ctrl Pts',(-1.33239425103724,-1.,1.63730653475089));
#26687=CARTESIAN_POINT('Ctrl Pts',(-1.33239425103724,1.,1.63730653475089));
#26688=CARTESIAN_POINT('Ctrl Pts',(-1.33368890676572,-1.,1.6434717485603));
#26689=CARTESIAN_POINT('Ctrl Pts',(-1.33368890676572,1.,1.6434717485603));
#26690=CARTESIAN_POINT('Ctrl Pts',(-1.33494590467993,-1.,1.6496563728683));
#26691=CARTESIAN_POINT('Ctrl Pts',(-1.33494590467993,1.,1.6496563728683));
#26692=CARTESIAN_POINT('Ctrl Pts',(-1.33616559745172,-1.,1.65586025952593));
#26693=CARTESIAN_POINT('Ctrl Pts',(-1.33616559745172,1.,1.65586025952593));
#26694=CARTESIAN_POINT('Ctrl Pts',(-1.33734820885262,-1.,1.66208312541983));
#26695=CARTESIAN_POINT('Ctrl Pts',(-1.33734820885262,1.,1.66208312541983));
#26696=CARTESIAN_POINT('Ctrl Pts',(-1.33849388654388,-1.,1.66832460783989));
#26697=CARTESIAN_POINT('Ctrl Pts',(-1.33849388654388,1.,1.66832460783989));
#26698=CARTESIAN_POINT('Ctrl Pts',(-1.3396027347034,-1.,1.67458429426086));
#26699=CARTESIAN_POINT('Ctrl Pts',(-1.3396027347034,1.,1.67458429426086));
#26700=CARTESIAN_POINT('Ctrl Pts',(-1.34067485185203,-1.,1.68086176030362));
#26701=CARTESIAN_POINT('Ctrl Pts',(-1.34067485185203,1.,1.68086176030362));
#26702=CARTESIAN_POINT('Ctrl Pts',(-1.341710374848,-1.,1.68715660868764));
#26703=CARTESIAN_POINT('Ctrl Pts',(-1.341710374848,1.,1.68715660868764));
#26704=CARTESIAN_POINT('Ctrl Pts',(-1.34270948206319,-1.,1.6934684849687));
#26705=CARTESIAN_POINT('Ctrl Pts',(-1.34270948206319,1.,1.6934684849687));
#26706=CARTESIAN_POINT('Ctrl Pts',(-1.34367237124483,-1.,1.69979707754427));
#26707=CARTESIAN_POINT('Ctrl Pts',(-1.34367237124483,1.,1.69979707754427));
#26708=CARTESIAN_POINT('Ctrl Pts',(-1.34459924533831,-1.,1.70614212266738));
#26709=CARTESIAN_POINT('Ctrl Pts',(-1.34459924533831,1.,1.70614212266738));
#26710=CARTESIAN_POINT('Ctrl Pts',(-1.34549029589416,-1.,1.71250340686822));
#26711=CARTESIAN_POINT('Ctrl Pts',(-1.34549029589416,1.,1.71250340686822));
#26712=CARTESIAN_POINT('Ctrl Pts',(-1.34634568653227,-1.,1.7188807715049));
#26713=CARTESIAN_POINT('Ctrl Pts',(-1.34634568653227,1.,1.7188807715049));
#26714=CARTESIAN_POINT('Ctrl Pts',(-1.34716554819527,-1.,1.72527410680674));
#26715=CARTESIAN_POINT('Ctrl Pts',(-1.34716554819527,1.,1.72527410680674));
#26716=CARTESIAN_POINT('Ctrl Pts',(-1.34779309152035,-1.,1.7304014965394));
#26717=CARTESIAN_POINT('Ctrl Pts',(-1.34779309152035,1.,1.7304014965394));
#26718=CARTESIAN_POINT('Ctrl Pts',(-1.34824783112887,-1.,1.73425417885907));
#26719=CARTESIAN_POINT('Ctrl Pts',(-1.34824783112887,1.,1.73425417885907));
#26720=CARTESIAN_POINT('Ctrl Pts',(-1.34854391898045,-1.,1.73682580585691));
#26721=CARTESIAN_POINT('Ctrl Pts',(-1.34854391898045,1.,1.73682580585691));
#26722=CARTESIAN_POINT('Ctrl Pts',(-1.34869019493419,-1.,1.73811241238545));
#26723=CARTESIAN_POINT('Ctrl Pts',(-1.34869019493419,1.,1.73811241238545));
#26724=CARTESIAN_POINT('',(-1.15624053661742,1.,1.31362392696032));
#26725=CARTESIAN_POINT('Ctrl Pts',(-1.15624053661742,1.,1.31362392696032));
#26726=CARTESIAN_POINT('Ctrl Pts',(-1.15950888730809,1.,1.31722977216397));
#26727=CARTESIAN_POINT('Ctrl Pts',(-1.16589330093588,1.,1.32428080721772));
#26728=CARTESIAN_POINT('Ctrl Pts',(-1.17501305789857,1.,1.33437539347008));
#26729=CARTESIAN_POINT('Ctrl Pts',(-1.18625865667441,1.,1.34687054001093));
#26730=CARTESIAN_POINT('Ctrl Pts',(-1.1987959077932,1.,1.36088705043885));
#26731=CARTESIAN_POINT('Ctrl Pts',(-1.20982812925645,1.,1.37331915607905));
#26732=CARTESIAN_POINT('Ctrl Pts',(-1.21938737280852,1.,1.38420564527715));
#26733=CARTESIAN_POINT('Ctrl Pts',(-1.22752961899387,1.,1.39361389568796));
#26734=CARTESIAN_POINT('Ctrl Pts',(-1.23434087290423,1.,1.40164708206106));
#26735=CARTESIAN_POINT('Ctrl Pts',(-1.23994455029534,1.,1.40845295531283));
#26736=CARTESIAN_POINT('Ctrl Pts',(-1.24450600513056,1.,1.41422913175179));
#26737=CARTESIAN_POINT('Ctrl Pts',(-1.24824430986571,1.,1.41923722596025));
#26738=CARTESIAN_POINT('Ctrl Pts',(-1.2514145557001,1.,1.42378102115575));
#26739=CARTESIAN_POINT('Ctrl Pts',(-1.25426945222639,1.,1.42815938799387));
#26740=CARTESIAN_POINT('Ctrl Pts',(-1.25702687965755,1.,1.43262645609691));
#26741=CARTESIAN_POINT('Ctrl Pts',(-1.25983531012005,1.,1.43734919180848));
#26742=CARTESIAN_POINT('Ctrl Pts',(-1.26273903323859,1.,1.44236470511303));
#26743=CARTESIAN_POINT('Ctrl Pts',(-1.26570925118868,1.,1.44761985001662));
#26744=CARTESIAN_POINT('Ctrl Pts',(-1.2686778680489,1.,1.45301422764247));
#26745=CARTESIAN_POINT('Ctrl Pts',(-1.27156805265289,1.,1.45843906294697));
#26746=CARTESIAN_POINT('Ctrl Pts',(-1.27433119897822,1.,1.46382431332476));
#26747=CARTESIAN_POINT('Ctrl Pts',(-1.27696414831089,1.,1.46916035917133));
#26748=CARTESIAN_POINT('Ctrl Pts',(-1.2794891824849,1.,1.4744717526707));
#26749=CARTESIAN_POINT('Ctrl Pts',(-1.28194158939517,1.,1.47980070347095));
#26750=CARTESIAN_POINT('Ctrl Pts',(-1.28435533880201,1.,1.4851881711891));
#26751=CARTESIAN_POINT('Ctrl Pts',(-1.2867467611644,1.,1.4906522831278));
#26752=CARTESIAN_POINT('Ctrl Pts',(-1.28911506584254,1.,1.49618896881754));
#26753=CARTESIAN_POINT('Ctrl Pts',(-1.29145022885181,1.,1.50178230149776));
#26754=CARTESIAN_POINT('Ctrl Pts',(-1.29373841372842,1.,1.50741159078365));
#26755=CARTESIAN_POINT('Ctrl Pts',(-1.29596850710509,1.,1.51305994241402));
#26756=CARTESIAN_POINT('Ctrl Pts',(-1.29813791800747,1.,1.51872184912724));
#26757=CARTESIAN_POINT('Ctrl Pts',(-1.30024984366328,1.,1.52439957861062));
#26758=CARTESIAN_POINT('Ctrl Pts',(-1.30231064395568,1.,1.53009970283891));
#26759=CARTESIAN_POINT('Ctrl Pts',(-1.30432735639489,1.,1.53582981268977));
#26760=CARTESIAN_POINT('Ctrl Pts',(-1.30630475189556,1.,1.54159462645432));
#26761=CARTESIAN_POINT('Ctrl Pts',(-1.30824393907473,1.,1.54739413957185));
#26762=CARTESIAN_POINT('Ctrl Pts',(-1.31014393684222,1.,1.55322568759481));
#26763=CARTESIAN_POINT('Ctrl Pts',(-1.31200264341696,1.,1.55908521254821));
#26764=CARTESIAN_POINT('Ctrl Pts',(-1.31381795281002,1.,1.56496872402353));
#26765=CARTESIAN_POINT('Ctrl Pts',(-1.31558903860016,1.,1.57087397835723));
#26766=CARTESIAN_POINT('Ctrl Pts',(-1.31731642317187,1.,1.5768005650559));
#26767=CARTESIAN_POINT('Ctrl Pts',(-1.31900135021432,1.,1.58274907898834));
#26768=CARTESIAN_POINT('Ctrl Pts',(-1.32064537110892,1.,1.58872057258245));
#26769=CARTESIAN_POINT('Ctrl Pts',(-1.32224985747682,1.,1.59471591079403));
#26770=CARTESIAN_POINT('Ctrl Pts',(-1.32381550858256,1.,1.60073511858687));
#26771=CARTESIAN_POINT('Ctrl Pts',(-1.32534250785782,1.,1.60677758290954));
#26772=CARTESIAN_POINT('Ctrl Pts',(-1.32683074483356,1.,1.6128423401575));
#26773=CARTESIAN_POINT('Ctrl Pts',(-1.32828000610449,1.,1.61892832270724));
#26774=CARTESIAN_POINT('Ctrl Pts',(-1.3296901950568,1.,1.62503464209797));
#26775=CARTESIAN_POINT('Ctrl Pts',(-1.33106149345645,1.,1.63116079730923));
#26776=CARTESIAN_POINT('Ctrl Pts',(-1.33239425103724,1.,1.63730653475089));
#26777=CARTESIAN_POINT('Ctrl Pts',(-1.33368890676572,1.,1.6434717485603));
#26778=CARTESIAN_POINT('Ctrl Pts',(-1.33494590467993,1.,1.6496563728683));
#26779=CARTESIAN_POINT('Ctrl Pts',(-1.33616559745172,1.,1.65586025952593));
#26780=CARTESIAN_POINT('Ctrl Pts',(-1.33734820885262,1.,1.66208312541983));
#26781=CARTESIAN_POINT('Ctrl Pts',(-1.33849388654388,1.,1.66832460783989));
#26782=CARTESIAN_POINT('Ctrl Pts',(-1.3396027347034,1.,1.67458429426086));
#26783=CARTESIAN_POINT('Ctrl Pts',(-1.34067485185203,1.,1.68086176030362));
#26784=CARTESIAN_POINT('Ctrl Pts',(-1.341710374848,1.,1.68715660868764));
#26785=CARTESIAN_POINT('Ctrl Pts',(-1.34270948206319,1.,1.6934684849687));
#26786=CARTESIAN_POINT('Ctrl Pts',(-1.34367237124483,1.,1.69979707754427));
#26787=CARTESIAN_POINT('Ctrl Pts',(-1.34459924533831,1.,1.70614212266738));
#26788=CARTESIAN_POINT('Ctrl Pts',(-1.34549029589416,1.,1.71250340686822));
#26789=CARTESIAN_POINT('Ctrl Pts',(-1.34634568653227,1.,1.7188807715049));
#26790=CARTESIAN_POINT('Ctrl Pts',(-1.34716554819527,1.,1.72527410680674));
#26791=CARTESIAN_POINT('Ctrl Pts',(-1.34779309152035,1.,1.7304014965394));
#26792=CARTESIAN_POINT('Ctrl Pts',(-1.34824783112887,1.,1.73425417885907));
#26793=CARTESIAN_POINT('Ctrl Pts',(-1.34854391898045,1.,1.73682580585691));
#26794=CARTESIAN_POINT('Ctrl Pts',(-1.34869019493419,1.,1.73811241238545));
#26795=CARTESIAN_POINT('',(-1.15624053661742,0.,1.31362392696032));
#26796=CARTESIAN_POINT('Origin',(0.,0.,0.));
#26797=CARTESIAN_POINT('',(-1.31362392696033,1.,1.15624053661742));
#26798=CARTESIAN_POINT('Origin',(0.,1.,0.));
#26799=CARTESIAN_POINT('',(-1.31362392696033,0.,1.15624053661742));
#26800=CARTESIAN_POINT('Ctrl Pts',(-1.73811241238545,-1.,1.34869019493419));
#26801=CARTESIAN_POINT('Ctrl Pts',(-1.73811241238545,1.,1.34869019493419));
#26802=CARTESIAN_POINT('Ctrl Pts',(-1.73682580585819,-1.,1.34854391898145));
#26803=CARTESIAN_POINT('Ctrl Pts',(-1.73682580585819,1.,1.34854391898145));
#26804=CARTESIAN_POINT('Ctrl Pts',(-1.73425417886255,-1.,1.34824783113158));
#26805=CARTESIAN_POINT('Ctrl Pts',(-1.73425417886255,1.,1.34824783113158));
#26806=CARTESIAN_POINT('Ctrl Pts',(-1.73040149654497,-1.,1.3477930915247));
#26807=CARTESIAN_POINT('Ctrl Pts',(-1.73040149654497,1.,1.3477930915247));
#26808=CARTESIAN_POINT('Ctrl Pts',(-1.72527410681298,-1.,1.34716554820013));
#26809=CARTESIAN_POINT('Ctrl Pts',(-1.72527410681298,1.,1.34716554820013));
#26810=CARTESIAN_POINT('Ctrl Pts',(-1.7188807715095,-1.,1.34634568653586));
#26811=CARTESIAN_POINT('Ctrl Pts',(-1.7188807715095,1.,1.34634568653586));
#26812=CARTESIAN_POINT('Ctrl Pts',(-1.71250340687011,-1.,1.34549029589563));
#26813=CARTESIAN_POINT('Ctrl Pts',(-1.71250340687011,1.,1.34549029589563));
#26814=CARTESIAN_POINT('Ctrl Pts',(-1.70614212266676,-1.,1.34459924533783));
#26815=CARTESIAN_POINT('Ctrl Pts',(-1.70614212266676,1.,1.34459924533783));
#26816=CARTESIAN_POINT('Ctrl Pts',(-1.69979707754221,-1.,1.34367237124322));
#26817=CARTESIAN_POINT('Ctrl Pts',(-1.69979707754221,1.,1.34367237124322));
#26818=CARTESIAN_POINT('Ctrl Pts',(-1.6934684849664,-1.,1.34270948206139));
#26819=CARTESIAN_POINT('Ctrl Pts',(-1.6934684849664,1.,1.34270948206139));
#26820=CARTESIAN_POINT('Ctrl Pts',(-1.68715660868602,-1.,1.34171037484673));
#26821=CARTESIAN_POINT('Ctrl Pts',(-1.68715660868602,1.,1.34171037484673));
#26822=CARTESIAN_POINT('Ctrl Pts',(-1.68086176030308,-1.,1.3406748518516));
#26823=CARTESIAN_POINT('Ctrl Pts',(-1.68086176030308,1.,1.3406748518516));
#26824=CARTESIAN_POINT('Ctrl Pts',(-1.67458429426126,-1.,1.33960273470372));
#26825=CARTESIAN_POINT('Ctrl Pts',(-1.67458429426126,1.,1.33960273470372));
#26826=CARTESIAN_POINT('Ctrl Pts',(-1.66832460784078,-1.,1.33849388654458));
#26827=CARTESIAN_POINT('Ctrl Pts',(-1.66832460784078,1.,1.33849388654458));
#26828=CARTESIAN_POINT('Ctrl Pts',(-1.66208312542073,-1.,1.33734820885331));
#26829=CARTESIAN_POINT('Ctrl Pts',(-1.66208312542073,1.,1.33734820885331));
#26830=CARTESIAN_POINT('Ctrl Pts',(-1.65586025952651,-1.,1.33616559745217));
#26831=CARTESIAN_POINT('Ctrl Pts',(-1.65586025952651,1.,1.33616559745217));
#26832=CARTESIAN_POINT('Ctrl Pts',(-1.64965637286843,-1.,1.33494590468003));
#26833=CARTESIAN_POINT('Ctrl Pts',(-1.64965637286843,1.,1.33494590468003));
#26834=CARTESIAN_POINT('Ctrl Pts',(-1.64347174856007,-1.,1.33368890676554));
#26835=CARTESIAN_POINT('Ctrl Pts',(-1.64347174856007,1.,1.33368890676554));
#26836=CARTESIAN_POINT('Ctrl Pts',(-1.6373065347505,-1.,1.33239425103694));
#26837=CARTESIAN_POINT('Ctrl Pts',(-1.6373065347505,1.,1.33239425103694));
#26838=CARTESIAN_POINT('Ctrl Pts',(-1.63116079730887,-1.,1.33106149345618));
#26839=CARTESIAN_POINT('Ctrl Pts',(-1.63116079730887,1.,1.33106149345618));
#26840=CARTESIAN_POINT('Ctrl Pts',(-1.62503464209777,-1.,1.32969019505665));
#26841=CARTESIAN_POINT('Ctrl Pts',(-1.62503464209777,1.,1.32969019505665));
#26842=CARTESIAN_POINT('Ctrl Pts',(-1.61892832270723,-1.,1.32828000610448));
#26843=CARTESIAN_POINT('Ctrl Pts',(-1.61892832270723,1.,1.32828000610448));
#26844=CARTESIAN_POINT('Ctrl Pts',(-1.61284234015762,-1.,1.32683074483365));
#26845=CARTESIAN_POINT('Ctrl Pts',(-1.61284234015762,1.,1.32683074483365));
#26846=CARTESIAN_POINT('Ctrl Pts',(-1.6067775829097,-1.,1.32534250785794));
#26847=CARTESIAN_POINT('Ctrl Pts',(-1.6067775829097,1.,1.32534250785794));
#26848=CARTESIAN_POINT('Ctrl Pts',(-1.600735118587,-1.,1.32381550858266));
#26849=CARTESIAN_POINT('Ctrl Pts',(-1.600735118587,1.,1.32381550858266));
#26850=CARTESIAN_POINT('Ctrl Pts',(-1.59471591079408,-1.,1.32224985747686));
#26851=CARTESIAN_POINT('Ctrl Pts',(-1.59471591079408,1.,1.32224985747686));
#26852=CARTESIAN_POINT('Ctrl Pts',(-1.58872057258244,-1.,1.32064537110891));
#26853=CARTESIAN_POINT('Ctrl Pts',(-1.58872057258244,1.,1.32064537110891));
#26854=CARTESIAN_POINT('Ctrl Pts',(-1.58274907898829,-1.,1.31900135021428));
#26855=CARTESIAN_POINT('Ctrl Pts',(-1.58274907898829,1.,1.31900135021428));
#26856=CARTESIAN_POINT('Ctrl Pts',(-1.57680056505585,-1.,1.31731642317183));
#26857=CARTESIAN_POINT('Ctrl Pts',(-1.57680056505585,1.,1.31731642317183));
#26858=CARTESIAN_POINT('Ctrl Pts',(-1.57087397835721,-1.,1.31558903860015));
#26859=CARTESIAN_POINT('Ctrl Pts',(-1.57087397835721,1.,1.31558903860015));
#26860=CARTESIAN_POINT('Ctrl Pts',(-1.56496872402352,-1.,1.31381795281002));
#26861=CARTESIAN_POINT('Ctrl Pts',(-1.56496872402352,1.,1.31381795281002));
#26862=CARTESIAN_POINT('Ctrl Pts',(-1.55908521254822,-1.,1.31200264341696));
#26863=CARTESIAN_POINT('Ctrl Pts',(-1.55908521254822,1.,1.31200264341696));
#26864=CARTESIAN_POINT('Ctrl Pts',(-1.55322568759481,-1.,1.31014393684221));
#26865=CARTESIAN_POINT('Ctrl Pts',(-1.55322568759481,1.,1.31014393684221));
#26866=CARTESIAN_POINT('Ctrl Pts',(-1.54739413957183,-1.,1.30824393907471));
#26867=CARTESIAN_POINT('Ctrl Pts',(-1.54739413957183,1.,1.30824393907471));
#26868=CARTESIAN_POINT('Ctrl Pts',(-1.54159462645428,-1.,1.30630475189553));
#26869=CARTESIAN_POINT('Ctrl Pts',(-1.54159462645428,1.,1.30630475189553));
#26870=CARTESIAN_POINT('Ctrl Pts',(-1.53582981268976,-1.,1.30432735639487));
#26871=CARTESIAN_POINT('Ctrl Pts',(-1.53582981268976,1.,1.30432735639487));
#26872=CARTESIAN_POINT('Ctrl Pts',(-1.53009970283893,-1.,1.3023106439557));
#26873=CARTESIAN_POINT('Ctrl Pts',(-1.53009970283893,1.,1.3023106439557));
#26874=CARTESIAN_POINT('Ctrl Pts',(-1.5243995786107,-1.,1.30024984366334));
#26875=CARTESIAN_POINT('Ctrl Pts',(-1.5243995786107,1.,1.30024984366334));
#26876=CARTESIAN_POINT('Ctrl Pts',(-1.51872184912735,-1.,1.29813791800757));
#26877=CARTESIAN_POINT('Ctrl Pts',(-1.51872184912735,1.,1.29813791800757));
#26878=CARTESIAN_POINT('Ctrl Pts',(-1.51305994241412,-1.,1.29596850710518));
#26879=CARTESIAN_POINT('Ctrl Pts',(-1.51305994241412,1.,1.29596850710518));
#26880=CARTESIAN_POINT('Ctrl Pts',(-1.50741159078367,-1.,1.29373841372843));
#26881=CARTESIAN_POINT('Ctrl Pts',(-1.50741159078367,1.,1.29373841372843));
#26882=CARTESIAN_POINT('Ctrl Pts',(-1.50178230149764,-1.,1.29145022885171));
#26883=CARTESIAN_POINT('Ctrl Pts',(-1.50178230149764,1.,1.29145022885171));
#26884=CARTESIAN_POINT('Ctrl Pts',(-1.49618896881729,-1.,1.28911506584232));
#26885=CARTESIAN_POINT('Ctrl Pts',(-1.49618896881729,1.,1.28911506584232));
#26886=CARTESIAN_POINT('Ctrl Pts',(-1.4906522831275,-1.,1.28674676116415));
#26887=CARTESIAN_POINT('Ctrl Pts',(-1.4906522831275,1.,1.28674676116415));
#26888=CARTESIAN_POINT('Ctrl Pts',(-1.48518817118891,-1.,1.28435533880184));
#26889=CARTESIAN_POINT('Ctrl Pts',(-1.48518817118891,1.,1.28435533880184));
#26890=CARTESIAN_POINT('Ctrl Pts',(-1.47980070347102,-1.,1.28194158939522));
#26891=CARTESIAN_POINT('Ctrl Pts',(-1.47980070347102,1.,1.28194158939522));
#26892=CARTESIAN_POINT('Ctrl Pts',(-1.4744717526711,-1.,1.27948918248524));
#26893=CARTESIAN_POINT('Ctrl Pts',(-1.4744717526711,1.,1.27948918248524));
#26894=CARTESIAN_POINT('Ctrl Pts',(-1.46916035917197,-1.,1.27696414831144));
#26895=CARTESIAN_POINT('Ctrl Pts',(-1.46916035917197,1.,1.27696414831144));
#26896=CARTESIAN_POINT('Ctrl Pts',(-1.4638243133254,-1.,1.27433119897877));
#26897=CARTESIAN_POINT('Ctrl Pts',(-1.4638243133254,1.,1.27433119897877));
#26898=CARTESIAN_POINT('Ctrl Pts',(-1.45843906294725,-1.,1.27156805265312));
#26899=CARTESIAN_POINT('Ctrl Pts',(-1.45843906294725,1.,1.27156805265312));
#26900=CARTESIAN_POINT('Ctrl Pts',(-1.45301422764205,-1.,1.26867786804854));
#26901=CARTESIAN_POINT('Ctrl Pts',(-1.45301422764205,1.,1.26867786804854));
#26902=CARTESIAN_POINT('Ctrl Pts',(-1.44761985001544,-1.,1.26570925118767));
#26903=CARTESIAN_POINT('Ctrl Pts',(-1.44761985001544,1.,1.26570925118767));
#26904=CARTESIAN_POINT('Ctrl Pts',(-1.44236470511145,-1.,1.26273903323723));
#26905=CARTESIAN_POINT('Ctrl Pts',(-1.44236470511145,1.,1.26273903323723));
#26906=CARTESIAN_POINT('Ctrl Pts',(-1.43734919180719,-1.,1.25983531011894));
#26907=CARTESIAN_POINT('Ctrl Pts',(-1.43734919180719,1.,1.25983531011894));
#26908=CARTESIAN_POINT('Ctrl Pts',(-1.43262645609679,-1.,1.25702687965744));
#26909=CARTESIAN_POINT('Ctrl Pts',(-1.43262645609679,1.,1.25702687965744));
#26910=CARTESIAN_POINT('Ctrl Pts',(-1.42815938799555,-1.,1.25426945222783));
#26911=CARTESIAN_POINT('Ctrl Pts',(-1.42815938799555,1.,1.25426945222783));
#26912=CARTESIAN_POINT('Ctrl Pts',(-1.42378102115911,-1.,1.25141455570299));
#26913=CARTESIAN_POINT('Ctrl Pts',(-1.42378102115911,1.,1.25141455570299));
#26914=CARTESIAN_POINT('Ctrl Pts',(-1.41923722596421,-1.,1.24824430986911));
#26915=CARTESIAN_POINT('Ctrl Pts',(-1.41923722596421,1.,1.24824430986911));
#26916=CARTESIAN_POINT('Ctrl Pts',(-1.41422913175437,-1.,1.24450600513278));
#26917=CARTESIAN_POINT('Ctrl Pts',(-1.41422913175437,1.,1.24450600513278));
#26918=CARTESIAN_POINT('Ctrl Pts',(-1.40845295531151,-1.,1.23994455029421));
#26919=CARTESIAN_POINT('Ctrl Pts',(-1.40845295531151,1.,1.23994455029421));
#26920=CARTESIAN_POINT('Ctrl Pts',(-1.40164708205345,-1.,1.23434087289768));
#26921=CARTESIAN_POINT('Ctrl Pts',(-1.40164708205345,1.,1.23434087289768));
#26922=CARTESIAN_POINT('Ctrl Pts',(-1.39361389567257,-1.,1.22752961898063));
#26923=CARTESIAN_POINT('Ctrl Pts',(-1.39361389567257,1.,1.22752961898063));
#26924=CARTESIAN_POINT('Ctrl Pts',(-1.38420564525391,-1.,1.21938737278853));
#26925=CARTESIAN_POINT('Ctrl Pts',(-1.38420564525391,1.,1.21938737278853));
#26926=CARTESIAN_POINT('Ctrl Pts',(-1.37331915604962,-1.,1.20982812923113));
#26927=CARTESIAN_POINT('Ctrl Pts',(-1.37331915604962,1.,1.20982812923113));
#26928=CARTESIAN_POINT('Ctrl Pts',(-1.36088705040677,-1.,1.1987959077656));
#26929=CARTESIAN_POINT('Ctrl Pts',(-1.36088705040677,1.,1.1987959077656));
#26930=CARTESIAN_POINT('Ctrl Pts',(-1.34687053998157,-1.,1.18625865664915));
#26931=CARTESIAN_POINT('Ctrl Pts',(-1.34687053998157,1.,1.18625865664915));
#26932=CARTESIAN_POINT('Ctrl Pts',(-1.33437539344842,-1.,1.17501305787994));
#26933=CARTESIAN_POINT('Ctrl Pts',(-1.33437539344842,1.,1.17501305787994));
#26934=CARTESIAN_POINT('Ctrl Pts',(-1.32428080720544,-1.,1.16589330092532));
#26935=CARTESIAN_POINT('Ctrl Pts',(-1.32428080720544,1.,1.16589330092532));
#26936=CARTESIAN_POINT('Ctrl Pts',(-1.3172297721596,-1.,1.15950888730433));
#26937=CARTESIAN_POINT('Ctrl Pts',(-1.3172297721596,1.,1.15950888730433));
#26938=CARTESIAN_POINT('Ctrl Pts',(-1.31362392696033,-1.,1.15624053661742));
#26939=CARTESIAN_POINT('Ctrl Pts',(-1.31362392696033,1.,1.15624053661742));
#26940=CARTESIAN_POINT('',(-1.73811241238545,1.,1.34869019493419));
#26941=CARTESIAN_POINT('Ctrl Pts',(-1.73811241238545,1.,1.34869019493419));
#26942=CARTESIAN_POINT('Ctrl Pts',(-1.73682580585819,1.,1.34854391898145));
#26943=CARTESIAN_POINT('Ctrl Pts',(-1.73425417886255,1.,1.34824783113158));
#26944=CARTESIAN_POINT('Ctrl Pts',(-1.73040149654497,1.,1.3477930915247));
#26945=CARTESIAN_POINT('Ctrl Pts',(-1.72527410681298,1.,1.34716554820013));
#26946=CARTESIAN_POINT('Ctrl Pts',(-1.7188807715095,1.,1.34634568653586));
#26947=CARTESIAN_POINT('Ctrl Pts',(-1.71250340687011,1.,1.34549029589563));
#26948=CARTESIAN_POINT('Ctrl Pts',(-1.70614212266676,1.,1.34459924533783));
#26949=CARTESIAN_POINT('Ctrl Pts',(-1.69979707754221,1.,1.34367237124322));
#26950=CARTESIAN_POINT('Ctrl Pts',(-1.6934684849664,1.,1.34270948206139));
#26951=CARTESIAN_POINT('Ctrl Pts',(-1.68715660868602,1.,1.34171037484673));
#26952=CARTESIAN_POINT('Ctrl Pts',(-1.68086176030308,1.,1.3406748518516));
#26953=CARTESIAN_POINT('Ctrl Pts',(-1.67458429426126,1.,1.33960273470372));
#26954=CARTESIAN_POINT('Ctrl Pts',(-1.66832460784078,1.,1.33849388654458));
#26955=CARTESIAN_POINT('Ctrl Pts',(-1.66208312542073,1.,1.33734820885331));
#26956=CARTESIAN_POINT('Ctrl Pts',(-1.65586025952651,1.,1.33616559745217));
#26957=CARTESIAN_POINT('Ctrl Pts',(-1.64965637286843,1.,1.33494590468003));
#26958=CARTESIAN_POINT('Ctrl Pts',(-1.64347174856007,1.,1.33368890676554));
#26959=CARTESIAN_POINT('Ctrl Pts',(-1.6373065347505,1.,1.33239425103694));
#26960=CARTESIAN_POINT('Ctrl Pts',(-1.63116079730887,1.,1.33106149345618));
#26961=CARTESIAN_POINT('Ctrl Pts',(-1.62503464209777,1.,1.32969019505665));
#26962=CARTESIAN_POINT('Ctrl Pts',(-1.61892832270723,1.,1.32828000610448));
#26963=CARTESIAN_POINT('Ctrl Pts',(-1.61284234015762,1.,1.32683074483365));
#26964=CARTESIAN_POINT('Ctrl Pts',(-1.6067775829097,1.,1.32534250785794));
#26965=CARTESIAN_POINT('Ctrl Pts',(-1.600735118587,1.,1.32381550858266));
#26966=CARTESIAN_POINT('Ctrl Pts',(-1.59471591079408,1.,1.32224985747686));
#26967=CARTESIAN_POINT('Ctrl Pts',(-1.58872057258244,1.,1.32064537110891));
#26968=CARTESIAN_POINT('Ctrl Pts',(-1.58274907898829,1.,1.31900135021428));
#26969=CARTESIAN_POINT('Ctrl Pts',(-1.57680056505585,1.,1.31731642317183));
#26970=CARTESIAN_POINT('Ctrl Pts',(-1.57087397835721,1.,1.31558903860015));
#26971=CARTESIAN_POINT('Ctrl Pts',(-1.56496872402352,1.,1.31381795281002));
#26972=CARTESIAN_POINT('Ctrl Pts',(-1.55908521254822,1.,1.31200264341696));
#26973=CARTESIAN_POINT('Ctrl Pts',(-1.55322568759481,1.,1.31014393684221));
#26974=CARTESIAN_POINT('Ctrl Pts',(-1.54739413957183,1.,1.30824393907471));
#26975=CARTESIAN_POINT('Ctrl Pts',(-1.54159462645428,1.,1.30630475189553));
#26976=CARTESIAN_POINT('Ctrl Pts',(-1.53582981268976,1.,1.30432735639487));
#26977=CARTESIAN_POINT('Ctrl Pts',(-1.53009970283893,1.,1.3023106439557));
#26978=CARTESIAN_POINT('Ctrl Pts',(-1.5243995786107,1.,1.30024984366334));
#26979=CARTESIAN_POINT('Ctrl Pts',(-1.51872184912735,1.,1.29813791800757));
#26980=CARTESIAN_POINT('Ctrl Pts',(-1.51305994241412,1.,1.29596850710518));
#26981=CARTESIAN_POINT('Ctrl Pts',(-1.50741159078367,1.,1.29373841372843));
#26982=CARTESIAN_POINT('Ctrl Pts',(-1.50178230149764,1.,1.29145022885171));
#26983=CARTESIAN_POINT('Ctrl Pts',(-1.49618896881729,1.,1.28911506584232));
#26984=CARTESIAN_POINT('Ctrl Pts',(-1.4906522831275,1.,1.28674676116415));
#26985=CARTESIAN_POINT('Ctrl Pts',(-1.48518817118891,1.,1.28435533880184));
#26986=CARTESIAN_POINT('Ctrl Pts',(-1.47980070347102,1.,1.28194158939522));
#26987=CARTESIAN_POINT('Ctrl Pts',(-1.4744717526711,1.,1.27948918248524));
#26988=CARTESIAN_POINT('Ctrl Pts',(-1.46916035917197,1.,1.27696414831144));
#26989=CARTESIAN_POINT('Ctrl Pts',(-1.4638243133254,1.,1.27433119897877));
#26990=CARTESIAN_POINT('Ctrl Pts',(-1.45843906294725,1.,1.27156805265312));
#26991=CARTESIAN_POINT('Ctrl Pts',(-1.45301422764205,1.,1.26867786804854));
#26992=CARTESIAN_POINT('Ctrl Pts',(-1.44761985001544,1.,1.26570925118767));
#26993=CARTESIAN_POINT('Ctrl Pts',(-1.44236470511145,1.,1.26273903323723));
#26994=CARTESIAN_POINT('Ctrl Pts',(-1.43734919180719,1.,1.25983531011894));
#26995=CARTESIAN_POINT('Ctrl Pts',(-1.43262645609679,1.,1.25702687965744));
#26996=CARTESIAN_POINT('Ctrl Pts',(-1.42815938799555,1.,1.25426945222783));
#26997=CARTESIAN_POINT('Ctrl Pts',(-1.42378102115911,1.,1.25141455570299));
#26998=CARTESIAN_POINT('Ctrl Pts',(-1.41923722596421,1.,1.24824430986911));
#26999=CARTESIAN_POINT('Ctrl Pts',(-1.41422913175437,1.,1.24450600513278));
#27000=CARTESIAN_POINT('Ctrl Pts',(-1.40845295531151,1.,1.23994455029421));
#27001=CARTESIAN_POINT('Ctrl Pts',(-1.40164708205345,1.,1.23434087289768));
#27002=CARTESIAN_POINT('Ctrl Pts',(-1.39361389567257,1.,1.22752961898063));
#27003=CARTESIAN_POINT('Ctrl Pts',(-1.38420564525391,1.,1.21938737278853));
#27004=CARTESIAN_POINT('Ctrl Pts',(-1.37331915604962,1.,1.20982812923113));
#27005=CARTESIAN_POINT('Ctrl Pts',(-1.36088705040677,1.,1.1987959077656));
#27006=CARTESIAN_POINT('Ctrl Pts',(-1.34687053998157,1.,1.18625865664915));
#27007=CARTESIAN_POINT('Ctrl Pts',(-1.33437539344842,1.,1.17501305787994));
#27008=CARTESIAN_POINT('Ctrl Pts',(-1.32428080720544,1.,1.16589330092532));
#27009=CARTESIAN_POINT('Ctrl Pts',(-1.3172297721596,1.,1.15950888730433));
#27010=CARTESIAN_POINT('Ctrl Pts',(-1.31362392696033,1.,1.15624053661742));
#27011=CARTESIAN_POINT('',(-1.73811241238545,0.,1.34869019493419));
#27012=CARTESIAN_POINT('Origin',(-1.81978687191668,0.,1.23627494547115));
#27013=CARTESIAN_POINT('',(-1.81978687191668,1.,1.23627494547115));
#27014=CARTESIAN_POINT('',(-1.73811241238545,1.,1.34869019493419));
#27015=CARTESIAN_POINT('',(-1.81978687191668,0.,1.23627494547115));
#27016=CARTESIAN_POINT('Ctrl Pts',(-1.5055822144029,-1.,0.892032620296855));
#27017=CARTESIAN_POINT('Ctrl Pts',(-1.5055822144029,1.,0.892032620296855));
#27018=CARTESIAN_POINT('Ctrl Pts',(-1.50980486807181,-1.,0.894452006967538));
#27019=CARTESIAN_POINT('Ctrl Pts',(-1.50980486807181,1.,0.894452006967538));
#27020=CARTESIAN_POINT('Ctrl Pts',(-1.51805569591479,-1.,0.89918504749193));
#27021=CARTESIAN_POINT('Ctrl Pts',(-1.51805569591479,1.,0.89918504749193));
#27022=CARTESIAN_POINT('Ctrl Pts',(-1.52984849890434,-1.,0.905967409640499));
#27023=CARTESIAN_POINT('Ctrl Pts',(-1.52984849890434,1.,0.905967409640499));
#27024=CARTESIAN_POINT('Ctrl Pts',(-1.54440491152808,-1.,0.91437591904658));
#27025=CARTESIAN_POINT('Ctrl Pts',(-1.54440491152808,1.,0.91437591904658));
#27026=CARTESIAN_POINT('Ctrl Pts',(-1.56065988582509,-1.,0.923832188966322));
#27027=CARTESIAN_POINT('Ctrl Pts',(-1.56065988582509,1.,0.923832188966322));
#27028=CARTESIAN_POINT('Ctrl Pts',(-1.57499388385561,-1.,0.932246680128849));
#27029=CARTESIAN_POINT('Ctrl Pts',(-1.57499388385561,1.,0.932246680128849));
#27030=CARTESIAN_POINT('Ctrl Pts',(-1.58744937489796,-1.,0.939646377909319));
#27031=CARTESIAN_POINT('Ctrl Pts',(-1.58744937489796,1.,0.939646377909319));
#27032=CARTESIAN_POINT('Ctrl Pts',(-1.59810042045408,-1.,0.946078063325796));
#27033=CARTESIAN_POINT('Ctrl Pts',(-1.59810042045408,1.,0.946078063325796));
#27034=CARTESIAN_POINT('Ctrl Pts',(-1.60706069897794,-1.,0.951613284361248));
#27035=CARTESIAN_POINT('Ctrl Pts',(-1.60706069897794,1.,0.951613284361248));
#27036=CARTESIAN_POINT('Ctrl Pts',(-1.61449324337233,-1.,0.956354422921573));
#27037=CARTESIAN_POINT('Ctrl Pts',(-1.61449324337233,1.,0.956354422921573));
#27038=CARTESIAN_POINT('Ctrl Pts',(-1.62061638139929,-1.,0.960438326099958));
#27039=CARTESIAN_POINT('Ctrl Pts',(-1.62061638139929,1.,0.960438326099958));
#27040=CARTESIAN_POINT('Ctrl Pts',(-1.6257193066974,-1.,0.964046107037821));
#27041=CARTESIAN_POINT('Ctrl Pts',(-1.6257193066974,1.,0.964046107037821));
#27042=CARTESIAN_POINT('Ctrl Pts',(-1.63013849959083,-1.,0.967387853228041));
#27043=CARTESIAN_POINT('Ctrl Pts',(-1.63013849959083,1.,0.967387853228041));
#27044=CARTESIAN_POINT('Ctrl Pts',(-1.63420665729609,-1.,0.970669715996356));
#27045=CARTESIAN_POINT('Ctrl Pts',(-1.63420665729609,1.,0.970669715996356));
#27046=CARTESIAN_POINT('Ctrl Pts',(-1.63820952658157,-1.,0.974066058287501));
#27047=CARTESIAN_POINT('Ctrl Pts',(-1.63820952658157,1.,0.974066058287501));
#27048=CARTESIAN_POINT('Ctrl Pts',(-1.64233990826831,-1.,0.977689794120297));
#27049=CARTESIAN_POINT('Ctrl Pts',(-1.64233990826831,1.,0.977689794120297));
#27050=CARTESIAN_POINT('Ctrl Pts',(-1.64665139190834,-1.,0.981562530940574));
#27051=CARTESIAN_POINT('Ctrl Pts',(-1.64665139190834,1.,0.981562530940574));
#27052=CARTESIAN_POINT('Ctrl Pts',(-1.6511001661277,-1.,0.985642622921626));
#27053=CARTESIAN_POINT('Ctrl Pts',(-1.6511001661277,1.,0.985642622921626));
#27054=CARTESIAN_POINT('Ctrl Pts',(-1.65559044289746,-1.,0.98985562785445));
#27055=CARTESIAN_POINT('Ctrl Pts',(-1.65559044289746,1.,0.98985562785445));
#27056=CARTESIAN_POINT('Ctrl Pts',(-1.66001553809916,-1.,0.994121836661116));
#27057=CARTESIAN_POINT('Ctrl Pts',(-1.66001553809916,1.,0.994121836661116));
#27058=CARTESIAN_POINT('Ctrl Pts',(-1.66430758030304,-1.,0.998389654952317));
#27059=CARTESIAN_POINT('Ctrl Pts',(-1.66430758030304,1.,0.998389654952317));
#27060=CARTESIAN_POINT('Ctrl Pts',(-1.66846059277231,-1.,1.00265091003682));
#27061=CARTESIAN_POINT('Ctrl Pts',(-1.66846059277231,1.,1.00265091003682));
#27062=CARTESIAN_POINT('Ctrl Pts',(-1.67250335383248,-1.,1.00692206696387));
#27063=CARTESIAN_POINT('Ctrl Pts',(-1.67250335383248,1.,1.00692206696387));
#27064=CARTESIAN_POINT('Ctrl Pts',(-1.67648246776457,-1.,1.01123236493507));
#27065=CARTESIAN_POINT('Ctrl Pts',(-1.67648246776457,1.,1.01123236493507));
#27066=CARTESIAN_POINT('Ctrl Pts',(-1.6804428989482,-1.,1.01561026162787));
#27067=CARTESIAN_POINT('Ctrl Pts',(-1.6804428989482,1.,1.01561026162787));
#27068=CARTESIAN_POINT('Ctrl Pts',(-1.68440578021739,-1.,1.02006795074222));
#27069=CARTESIAN_POINT('Ctrl Pts',(-1.68440578021739,1.,1.02006795074222));
#27070=CARTESIAN_POINT('Ctrl Pts',(-1.68836910178475,-1.,1.02460180535272));
#27071=CARTESIAN_POINT('Ctrl Pts',(-1.68836910178475,1.,1.02460180535272));
#27072=CARTESIAN_POINT('Ctrl Pts',(-1.69231840863471,-1.,1.02919977579155));
#27073=CARTESIAN_POINT('Ctrl Pts',(-1.69231840863471,1.,1.02919977579155));
#27074=CARTESIAN_POINT('Ctrl Pts',(-1.69623414782769,-1.,1.03384646003587));
#27075=CARTESIAN_POINT('Ctrl Pts',(-1.69623414782769,1.,1.03384646003587));
#27076=CARTESIAN_POINT('Ctrl Pts',(-1.70010052930951,-1.,1.03852922490782));
#27077=CARTESIAN_POINT('Ctrl Pts',(-1.70010052930951,1.,1.03852922490782));
#27078=CARTESIAN_POINT('Ctrl Pts',(-1.70391338707969,-1.,1.04324363334546));
#27079=CARTESIAN_POINT('Ctrl Pts',(-1.70391338707969,1.,1.04324363334546));
#27080=CARTESIAN_POINT('Ctrl Pts',(-1.70767646263641,-1.,1.0479908540499));
#27081=CARTESIAN_POINT('Ctrl Pts',(-1.70767646263641,1.,1.0479908540499));
#27082=CARTESIAN_POINT('Ctrl Pts',(-1.71139783543986,-1.,1.05277517202854));
#27083=CARTESIAN_POINT('Ctrl Pts',(-1.71139783543986,1.,1.05277517202854));
#27084=CARTESIAN_POINT('Ctrl Pts',(-1.71508654427022,-1.,1.05760163192481));
#27085=CARTESIAN_POINT('Ctrl Pts',(-1.71508654427022,1.,1.05760163192481));
#27086=CARTESIAN_POINT('Ctrl Pts',(-1.71874858456908,-1.,1.0624732468065));
#27087=CARTESIAN_POINT('Ctrl Pts',(-1.71874858456908,1.,1.0624732468065));
#27088=CARTESIAN_POINT('Ctrl Pts',(-1.72238500928456,-1.,1.06738966975463));
#27089=CARTESIAN_POINT('Ctrl Pts',(-1.72238500928456,1.,1.06738966975463));
#27090=CARTESIAN_POINT('Ctrl Pts',(-1.72599406198489,-1.,1.07234866990252));
#27091=CARTESIAN_POINT('Ctrl Pts',(-1.72599406198489,1.,1.07234866990252));
#27092=CARTESIAN_POINT('Ctrl Pts',(-1.72957248977424,-1.,1.0773470373727));
#27093=CARTESIAN_POINT('Ctrl Pts',(-1.72957248977424,1.,1.0773470373727));
#27094=CARTESIAN_POINT('Ctrl Pts',(-1.73311705663407,-1.,1.08238162784749));
#27095=CARTESIAN_POINT('Ctrl Pts',(-1.73311705663407,1.,1.08238162784749));
#27096=CARTESIAN_POINT('Ctrl Pts',(-1.73662628326093,-1.,1.08745056285429));
#27097=CARTESIAN_POINT('Ctrl Pts',(-1.73662628326093,1.,1.08745056285429));
#27098=CARTESIAN_POINT('Ctrl Pts',(-1.74010053962252,-1.,1.09255329056496));
#27099=CARTESIAN_POINT('Ctrl Pts',(-1.74010053962252,1.,1.09255329056496));
#27100=CARTESIAN_POINT('Ctrl Pts',(-1.74354119236212,-1.,1.09768999241229));
#27101=CARTESIAN_POINT('Ctrl Pts',(-1.74354119236212,1.,1.09768999241229));
#27102=CARTESIAN_POINT('Ctrl Pts',(-1.74695004214924,-1.,1.10286118991144));
#27103=CARTESIAN_POINT('Ctrl Pts',(-1.74695004214924,1.,1.10286118991144));
#27104=CARTESIAN_POINT('Ctrl Pts',(-1.75032866075914,-1.,1.10806728183003));
#27105=CARTESIAN_POINT('Ctrl Pts',(-1.75032866075914,1.,1.10806728183003));
#27106=CARTESIAN_POINT('Ctrl Pts',(-1.75367772094617,-1.,1.11330807582542));
#27107=CARTESIAN_POINT('Ctrl Pts',(-1.75367772094617,1.,1.11330807582542));
#27108=CARTESIAN_POINT('Ctrl Pts',(-1.75699720772089,-1.,1.11858293216752));
#27109=CARTESIAN_POINT('Ctrl Pts',(-1.75699720772089,1.,1.11858293216752));
#27110=CARTESIAN_POINT('Ctrl Pts',(-1.76028671825084,-1.,1.12389096855078));
#27111=CARTESIAN_POINT('Ctrl Pts',(-1.76028671825084,1.,1.12389096855078));
#27112=CARTESIAN_POINT('Ctrl Pts',(-1.76354571966171,-1.,1.12923123555076));
#27113=CARTESIAN_POINT('Ctrl Pts',(-1.76354571966171,1.,1.12923123555076));
#27114=CARTESIAN_POINT('Ctrl Pts',(-1.76677384551883,-1.,1.13460291804635));
#27115=CARTESIAN_POINT('Ctrl Pts',(-1.76677384551883,1.,1.13460291804635));
#27116=CARTESIAN_POINT('Ctrl Pts',(-1.76997111386806,-1.,1.14000548337));
#27117=CARTESIAN_POINT('Ctrl Pts',(-1.76997111386806,1.,1.14000548337));
#27118=CARTESIAN_POINT('Ctrl Pts',(-1.77313777896234,-1.,1.14543858226948));
#27119=CARTESIAN_POINT('Ctrl Pts',(-1.77313777896234,1.,1.14543858226948));
#27120=CARTESIAN_POINT('Ctrl Pts',(-1.77627422557034,-1.,1.15090197841531));
#27121=CARTESIAN_POINT('Ctrl Pts',(-1.77627422557034,1.,1.15090197841531));
#27122=CARTESIAN_POINT('Ctrl Pts',(-1.77938085564261,-1.,1.15639547194689));
#27123=CARTESIAN_POINT('Ctrl Pts',(-1.77938085564261,1.,1.15639547194689));
#27124=CARTESIAN_POINT('Ctrl Pts',(-1.78245795880949,-1.,1.16191881298458));
#27125=CARTESIAN_POINT('Ctrl Pts',(-1.78245795880949,1.,1.16191881298458));
#27126=CARTESIAN_POINT('Ctrl Pts',(-1.78550566040349,-1.,1.16747166312239));
#27127=CARTESIAN_POINT('Ctrl Pts',(-1.78550566040349,1.,1.16747166312239));
#27128=CARTESIAN_POINT('Ctrl Pts',(-1.78852398877523,-1.,1.17305363177265));
#27129=CARTESIAN_POINT('Ctrl Pts',(-1.78852398877523,1.,1.17305363177265));
#27130=CARTESIAN_POINT('Ctrl Pts',(-1.79151291552646,-1.,1.17866429440781));
#27131=CARTESIAN_POINT('Ctrl Pts',(-1.79151291552646,1.,1.17866429440781));
#27132=CARTESIAN_POINT('Ctrl Pts',(-1.79447240321572,-1.,1.18430321697471));
#27133=CARTESIAN_POINT('Ctrl Pts',(-1.79447240321572,1.,1.18430321697471));
#27134=CARTESIAN_POINT('Ctrl Pts',(-1.79740245923649,-1.,1.1899699793456));
#27135=CARTESIAN_POINT('Ctrl Pts',(-1.79740245923649,1.,1.1899699793456));
#27136=CARTESIAN_POINT('Ctrl Pts',(-1.80030314370121,-1.,1.19566418930405));
#27137=CARTESIAN_POINT('Ctrl Pts',(-1.80030314370121,1.,1.19566418930405));
#27138=CARTESIAN_POINT('Ctrl Pts',(-1.8031745483882,-1.,1.2013854893912));
#27139=CARTESIAN_POINT('Ctrl Pts',(-1.8031745483882,1.,1.2013854893912));
#27140=CARTESIAN_POINT('Ctrl Pts',(-1.80601678480772,-1.,1.20713356605519));
#27141=CARTESIAN_POINT('Ctrl Pts',(-1.80601678480772,1.,1.20713356605519));
#27142=CARTESIAN_POINT('Ctrl Pts',(-1.80882996916931,-1.,1.2129081570818));
#27143=CARTESIAN_POINT('Ctrl Pts',(-1.80882996916931,1.,1.2129081570818));
#27144=CARTESIAN_POINT('Ctrl Pts',(-1.81161420806172,-1.,1.2187090610323));
#27145=CARTESIAN_POINT('Ctrl Pts',(-1.81161420806172,1.,1.2187090610323));
#27146=CARTESIAN_POINT('Ctrl Pts',(-1.81436959209778,-1.,1.22453613304507));
#27147=CARTESIAN_POINT('Ctrl Pts',(-1.81436959209778,1.,1.22453613304507));
#27148=CARTESIAN_POINT('Ctrl Pts',(-1.81655087183054,-1.,1.22921864890975));
#27149=CARTESIAN_POINT('Ctrl Pts',(-1.81655087183054,1.,1.22921864890975));
#27150=CARTESIAN_POINT('Ctrl Pts',(-1.81817389920914,-1.,1.23274224526804));
#27151=CARTESIAN_POINT('Ctrl Pts',(-1.81817389920914,1.,1.23274224526804));
#27152=CARTESIAN_POINT('Ctrl Pts',(-1.81925017193531,-1.,1.23509651170384));
#27153=CARTESIAN_POINT('Ctrl Pts',(-1.81925017193531,1.,1.23509651170384));
#27154=CARTESIAN_POINT('Ctrl Pts',(-1.81978687191668,-1.,1.23627494547115));
#27155=CARTESIAN_POINT('Ctrl Pts',(-1.81978687191668,1.,1.23627494547115));
#27156=CARTESIAN_POINT('',(-1.5055822144029,1.,0.892032620296855));
#27157=CARTESIAN_POINT('Ctrl Pts',(-1.5055822144029,1.,0.892032620296855));
#27158=CARTESIAN_POINT('Ctrl Pts',(-1.50980486807181,1.,0.894452006967538));
#27159=CARTESIAN_POINT('Ctrl Pts',(-1.51805569591479,1.,0.89918504749193));
#27160=CARTESIAN_POINT('Ctrl Pts',(-1.52984849890434,1.,0.905967409640499));
#27161=CARTESIAN_POINT('Ctrl Pts',(-1.54440491152808,1.,0.91437591904658));
#27162=CARTESIAN_POINT('Ctrl Pts',(-1.56065988582509,1.,0.923832188966322));
#27163=CARTESIAN_POINT('Ctrl Pts',(-1.57499388385561,1.,0.932246680128849));
#27164=CARTESIAN_POINT('Ctrl Pts',(-1.58744937489796,1.,0.939646377909319));
#27165=CARTESIAN_POINT('Ctrl Pts',(-1.59810042045408,1.,0.946078063325796));
#27166=CARTESIAN_POINT('Ctrl Pts',(-1.60706069897794,1.,0.951613284361248));
#27167=CARTESIAN_POINT('Ctrl Pts',(-1.61449324337233,1.,0.956354422921573));
#27168=CARTESIAN_POINT('Ctrl Pts',(-1.62061638139929,1.,0.960438326099958));
#27169=CARTESIAN_POINT('Ctrl Pts',(-1.6257193066974,1.,0.964046107037821));
#27170=CARTESIAN_POINT('Ctrl Pts',(-1.63013849959083,1.,0.967387853228041));
#27171=CARTESIAN_POINT('Ctrl Pts',(-1.63420665729609,1.,0.970669715996356));
#27172=CARTESIAN_POINT('Ctrl Pts',(-1.63820952658157,1.,0.974066058287501));
#27173=CARTESIAN_POINT('Ctrl Pts',(-1.64233990826831,1.,0.977689794120297));
#27174=CARTESIAN_POINT('Ctrl Pts',(-1.64665139190834,1.,0.981562530940574));
#27175=CARTESIAN_POINT('Ctrl Pts',(-1.6511001661277,1.,0.985642622921626));
#27176=CARTESIAN_POINT('Ctrl Pts',(-1.65559044289746,1.,0.98985562785445));
#27177=CARTESIAN_POINT('Ctrl Pts',(-1.66001553809916,1.,0.994121836661116));
#27178=CARTESIAN_POINT('Ctrl Pts',(-1.66430758030304,1.,0.998389654952317));
#27179=CARTESIAN_POINT('Ctrl Pts',(-1.66846059277231,1.,1.00265091003682));
#27180=CARTESIAN_POINT('Ctrl Pts',(-1.67250335383248,1.,1.00692206696387));
#27181=CARTESIAN_POINT('Ctrl Pts',(-1.67648246776457,1.,1.01123236493507));
#27182=CARTESIAN_POINT('Ctrl Pts',(-1.6804428989482,1.,1.01561026162787));
#27183=CARTESIAN_POINT('Ctrl Pts',(-1.68440578021739,1.,1.02006795074222));
#27184=CARTESIAN_POINT('Ctrl Pts',(-1.68836910178475,1.,1.02460180535272));
#27185=CARTESIAN_POINT('Ctrl Pts',(-1.69231840863471,1.,1.02919977579155));
#27186=CARTESIAN_POINT('Ctrl Pts',(-1.69623414782769,1.,1.03384646003587));
#27187=CARTESIAN_POINT('Ctrl Pts',(-1.70010052930951,1.,1.03852922490782));
#27188=CARTESIAN_POINT('Ctrl Pts',(-1.70391338707969,1.,1.04324363334546));
#27189=CARTESIAN_POINT('Ctrl Pts',(-1.70767646263641,1.,1.0479908540499));
#27190=CARTESIAN_POINT('Ctrl Pts',(-1.71139783543986,1.,1.05277517202854));
#27191=CARTESIAN_POINT('Ctrl Pts',(-1.71508654427022,1.,1.05760163192481));
#27192=CARTESIAN_POINT('Ctrl Pts',(-1.71874858456908,1.,1.0624732468065));
#27193=CARTESIAN_POINT('Ctrl Pts',(-1.72238500928456,1.,1.06738966975463));
#27194=CARTESIAN_POINT('Ctrl Pts',(-1.72599406198489,1.,1.07234866990252));
#27195=CARTESIAN_POINT('Ctrl Pts',(-1.72957248977424,1.,1.0773470373727));
#27196=CARTESIAN_POINT('Ctrl Pts',(-1.73311705663407,1.,1.08238162784749));
#27197=CARTESIAN_POINT('Ctrl Pts',(-1.73662628326093,1.,1.08745056285429));
#27198=CARTESIAN_POINT('Ctrl Pts',(-1.74010053962252,1.,1.09255329056496));
#27199=CARTESIAN_POINT('Ctrl Pts',(-1.74354119236212,1.,1.09768999241229));
#27200=CARTESIAN_POINT('Ctrl Pts',(-1.74695004214924,1.,1.10286118991144));
#27201=CARTESIAN_POINT('Ctrl Pts',(-1.75032866075914,1.,1.10806728183003));
#27202=CARTESIAN_POINT('Ctrl Pts',(-1.75367772094617,1.,1.11330807582542));
#27203=CARTESIAN_POINT('Ctrl Pts',(-1.75699720772089,1.,1.11858293216752));
#27204=CARTESIAN_POINT('Ctrl Pts',(-1.76028671825084,1.,1.12389096855078));
#27205=CARTESIAN_POINT('Ctrl Pts',(-1.76354571966171,1.,1.12923123555076));
#27206=CARTESIAN_POINT('Ctrl Pts',(-1.76677384551883,1.,1.13460291804635));
#27207=CARTESIAN_POINT('Ctrl Pts',(-1.76997111386806,1.,1.14000548337));
#27208=CARTESIAN_POINT('Ctrl Pts',(-1.77313777896234,1.,1.14543858226948));
#27209=CARTESIAN_POINT('Ctrl Pts',(-1.77627422557034,1.,1.15090197841531));
#27210=CARTESIAN_POINT('Ctrl Pts',(-1.77938085564261,1.,1.15639547194689));
#27211=CARTESIAN_POINT('Ctrl Pts',(-1.78245795880949,1.,1.16191881298458));
#27212=CARTESIAN_POINT('Ctrl Pts',(-1.78550566040349,1.,1.16747166312239));
#27213=CARTESIAN_POINT('Ctrl Pts',(-1.78852398877523,1.,1.17305363177265));
#27214=CARTESIAN_POINT('Ctrl Pts',(-1.79151291552646,1.,1.17866429440781));
#27215=CARTESIAN_POINT('Ctrl Pts',(-1.79447240321572,1.,1.18430321697471));
#27216=CARTESIAN_POINT('Ctrl Pts',(-1.79740245923649,1.,1.1899699793456));
#27217=CARTESIAN_POINT('Ctrl Pts',(-1.80030314370121,1.,1.19566418930405));
#27218=CARTESIAN_POINT('Ctrl Pts',(-1.8031745483882,1.,1.2013854893912));
#27219=CARTESIAN_POINT('Ctrl Pts',(-1.80601678480772,1.,1.20713356605519));
#27220=CARTESIAN_POINT('Ctrl Pts',(-1.80882996916931,1.,1.2129081570818));
#27221=CARTESIAN_POINT('Ctrl Pts',(-1.81161420806172,1.,1.2187090610323));
#27222=CARTESIAN_POINT('Ctrl Pts',(-1.81436959209778,1.,1.22453613304507));
#27223=CARTESIAN_POINT('Ctrl Pts',(-1.81655087183054,1.,1.22921864890975));
#27224=CARTESIAN_POINT('Ctrl Pts',(-1.81817389920914,1.,1.23274224526804));
#27225=CARTESIAN_POINT('Ctrl Pts',(-1.81925017193531,1.,1.23509651170384));
#27226=CARTESIAN_POINT('Ctrl Pts',(-1.81978687191668,1.,1.23627494547115));
#27227=CARTESIAN_POINT('',(-1.5055822144029,0.,0.892032620296856));
#27228=CARTESIAN_POINT('Origin',(0.,0.,0.));
#27229=CARTESIAN_POINT('',(-1.60662857109684,1.,0.693717979106305));
#27230=CARTESIAN_POINT('Origin',(0.,1.,0.));
#27231=CARTESIAN_POINT('',(-1.60662857109684,0.,0.693717979106306));
#27232=CARTESIAN_POINT('Ctrl Pts',(-2.0698113262342,-1.,0.7455743247944));
#27233=CARTESIAN_POINT('Ctrl Pts',(-2.0698113262342,1.,0.7455743247944));
#27234=CARTESIAN_POINT('Ctrl Pts',(-2.06854248895728,-1.,0.745832791378367));
#27235=CARTESIAN_POINT('Ctrl Pts',(-2.06854248895728,1.,0.745832791378367));
#27236=CARTESIAN_POINT('Ctrl Pts',(-2.06600523016815,-1.,0.7463458715442));
#27237=CARTESIAN_POINT('Ctrl Pts',(-2.06600523016815,1.,0.7463458715442));
#27238=CARTESIAN_POINT('Ctrl Pts',(-2.06220058927826,-1.,0.747103932787919));
#27239=CARTESIAN_POINT('Ctrl Pts',(-2.06220058927826,1.,0.747103932787919));
#27240=CARTESIAN_POINT('Ctrl Pts',(-2.05713023031006,-1.,0.748091554183802));
#27241=CARTESIAN_POINT('Ctrl Pts',(-2.05713023031006,1.,0.748091554183802));
#27242=CARTESIAN_POINT('Ctrl Pts',(-2.05079645592154,-1.,0.749287468665046));
#27243=CARTESIAN_POINT('Ctrl Pts',(-2.05079645592154,1.,0.749287468665046));
#27244=CARTESIAN_POINT('Ctrl Pts',(-2.04446689147979,-1.,0.750444657875576));
#27245=CARTESIAN_POINT('Ctrl Pts',(-2.04446689147979,1.,0.750444657875576));
#27246=CARTESIAN_POINT('Ctrl Pts',(-2.03814160092099,-1.,0.751562963361115));
#27247=CARTESIAN_POINT('Ctrl Pts',(-2.03814160092099,1.,0.751562963361115));
#27248=CARTESIAN_POINT('Ctrl Pts',(-2.03182068456221,-1.,0.752642180487211));
#27249=CARTESIAN_POINT('Ctrl Pts',(-2.03182068456221,1.,0.752642180487211));
#27250=CARTESIAN_POINT('Ctrl Pts',(-2.02550428623313,-1.,0.753682061112768));
#27251=CARTESIAN_POINT('Ctrl Pts',(-2.02550428623313,1.,0.753682061112768));
#27252=CARTESIAN_POINT('Ctrl Pts',(-2.01919259405809,-1.,0.754682330722816));
#27253=CARTESIAN_POINT('Ctrl Pts',(-2.01919259405809,1.,0.754682330722816));
#27254=CARTESIAN_POINT('Ctrl Pts',(-2.01288584328084,-1.,0.755642704957865));
#27255=CARTESIAN_POINT('Ctrl Pts',(-2.01288584328084,1.,0.755642704957865));
#27256=CARTESIAN_POINT('Ctrl Pts',(-2.0065843158773,-1.,0.75656290464667));
#27257=CARTESIAN_POINT('Ctrl Pts',(-2.0065843158773,1.,0.75656290464667));
#27258=CARTESIAN_POINT('Ctrl Pts',(-2.00028834739178,-1.,0.757442676862724));
#27259=CARTESIAN_POINT('Ctrl Pts',(-2.00028834739178,1.,0.757442676862724));
#27260=CARTESIAN_POINT('Ctrl Pts',(-1.99399831098817,-1.,0.758281796766761));
#27261=CARTESIAN_POINT('Ctrl Pts',(-1.99399831098817,1.,0.758281796766761));
#27262=CARTESIAN_POINT('Ctrl Pts',(-1.98771456680874,-1.,0.759080037802488));
#27263=CARTESIAN_POINT('Ctrl Pts',(-1.98771456680874,1.,0.759080037802488));
#27264=CARTESIAN_POINT('Ctrl Pts',(-1.98143741418172,-1.,0.75983714745219));
#27265=CARTESIAN_POINT('Ctrl Pts',(-1.98143741418172,1.,0.75983714745219));
#27266=CARTESIAN_POINT('Ctrl Pts',(-1.97516705321494,-1.,0.760552825409757));
#27267=CARTESIAN_POINT('Ctrl Pts',(-1.97516705321494,1.,0.760552825409757));
#27268=CARTESIAN_POINT('Ctrl Pts',(-1.96890351582499,-1.,0.76122669048382));
#27269=CARTESIAN_POINT('Ctrl Pts',(-1.96890351582499,1.,0.76122669048382));
#27270=CARTESIAN_POINT('Ctrl Pts',(-1.96264672744186,-1.,0.761858300014423));
#27271=CARTESIAN_POINT('Ctrl Pts',(-1.96264672744186,1.,0.761858300014423));
#27272=CARTESIAN_POINT('Ctrl Pts',(-1.95639665309869,-1.,0.762447203806179));
#27273=CARTESIAN_POINT('Ctrl Pts',(-1.95639665309869,1.,0.762447203806179));
#27274=CARTESIAN_POINT('Ctrl Pts',(-1.95015342590024,-1.,0.762992990878769));
#27275=CARTESIAN_POINT('Ctrl Pts',(-1.95015342590024,1.,0.762992990878769));
#27276=CARTESIAN_POINT('Ctrl Pts',(-1.9439174661764,-1.,0.763495333538629));
#27277=CARTESIAN_POINT('Ctrl Pts',(-1.9439174661764,1.,0.763495333538629));
#27278=CARTESIAN_POINT('Ctrl Pts',(-1.93768964875886,-1.,0.763954049121458));
#27279=CARTESIAN_POINT('Ctrl Pts',(-1.93768964875886,1.,0.763954049121458));
#27280=CARTESIAN_POINT('Ctrl Pts',(-1.93147105496382,-1.,0.76436901067394));
#27281=CARTESIAN_POINT('Ctrl Pts',(-1.93147105496382,1.,0.76436901067394));
#27282=CARTESIAN_POINT('Ctrl Pts',(-1.92526263537048,-1.,0.764740025488211));
#27283=CARTESIAN_POINT('Ctrl Pts',(-1.92526263537048,1.,0.764740025488211));
#27284=CARTESIAN_POINT('Ctrl Pts',(-1.91906491634196,-1.,0.765066729667088));
#27285=CARTESIAN_POINT('Ctrl Pts',(-1.91906491634196,1.,0.765066729667088));
#27286=CARTESIAN_POINT('Ctrl Pts',(-1.91287765805169,-1.,0.765348465884722));
#27287=CARTESIAN_POINT('Ctrl Pts',(-1.91287765805169,1.,0.765348465884722));
#27288=CARTESIAN_POINT('Ctrl Pts',(-1.90669961402356,-1.,0.765584196937919));
#27289=CARTESIAN_POINT('Ctrl Pts',(-1.90669961402356,1.,0.765584196937919));
#27290=CARTESIAN_POINT('Ctrl Pts',(-1.90052930393596,-1.,0.765772772593386));
#27291=CARTESIAN_POINT('Ctrl Pts',(-1.90052930393596,1.,0.765772772593386));
#27292=CARTESIAN_POINT('Ctrl Pts',(-1.89436577771388,-1.,0.765913193856978));
#27293=CARTESIAN_POINT('Ctrl Pts',(-1.89436577771388,1.,0.765913193856978));
#27294=CARTESIAN_POINT('Ctrl Pts',(-1.88820926433409,-1.,0.766004837062091));
#27295=CARTESIAN_POINT('Ctrl Pts',(-1.88820926433409,1.,0.766004837062091));
#27296=CARTESIAN_POINT('Ctrl Pts',(-1.88206215302561,-1.,0.766047794851864));
#27297=CARTESIAN_POINT('Ctrl Pts',(-1.88206215302561,1.,0.766047794851864));
#27298=CARTESIAN_POINT('Ctrl Pts',(-1.87592888967883,-1.,0.766042837036744));
#27299=CARTESIAN_POINT('Ctrl Pts',(-1.87592888967883,1.,0.766042837036744));
#27300=CARTESIAN_POINT('Ctrl Pts',(-1.86981398314341,-1.,0.765990708546091));
#27301=CARTESIAN_POINT('Ctrl Pts',(-1.86981398314341,1.,0.765990708546091));
#27302=CARTESIAN_POINT('Ctrl Pts',(-1.86372027063312,-1.,0.765891519092547));
#27303=CARTESIAN_POINT('Ctrl Pts',(-1.86372027063312,1.,0.765891519092547));
#27304=CARTESIAN_POINT('Ctrl Pts',(-1.85764741390394,-1.,0.765744212909318));
#27305=CARTESIAN_POINT('Ctrl Pts',(-1.85764741390394,1.,0.765744212909318));
#27306=CARTESIAN_POINT('Ctrl Pts',(-1.85158945130063,-1.,0.765545710619062));
#27307=CARTESIAN_POINT('Ctrl Pts',(-1.85158945130063,1.,0.765545710619062));
#27308=CARTESIAN_POINT('Ctrl Pts',(-1.84553698875924,-1.,0.765291664862029));
#27309=CARTESIAN_POINT('Ctrl Pts',(-1.84553698875924,1.,0.765291664862029));
#27310=CARTESIAN_POINT('Ctrl Pts',(-1.83948181064835,-1.,0.764978057881737));
#27311=CARTESIAN_POINT('Ctrl Pts',(-1.83948181064835,1.,0.764978057881737));
#27312=CARTESIAN_POINT('Ctrl Pts',(-1.83342077227142,-1.,0.764602549687853));
#27313=CARTESIAN_POINT('Ctrl Pts',(-1.83342077227142,1.,0.764602549687853));
#27314=CARTESIAN_POINT('Ctrl Pts',(-1.82735991200065,-1.,0.764165902605995));
#27315=CARTESIAN_POINT('Ctrl Pts',(-1.82735991200065,1.,0.764165902605995));
#27316=CARTESIAN_POINT('Ctrl Pts',(-1.82131873145266,-1.,0.763673465462726));
#27317=CARTESIAN_POINT('Ctrl Pts',(-1.82131873145266,1.,0.763673465462726));
#27318=CARTESIAN_POINT('Ctrl Pts',(-1.8153211840553,-1.,0.763132003836634));
#27319=CARTESIAN_POINT('Ctrl Pts',(-1.8153211840553,1.,0.763132003836634));
#27320=CARTESIAN_POINT('Ctrl Pts',(-1.80938551463965,-1.,0.762546129463938));
#27321=CARTESIAN_POINT('Ctrl Pts',(-1.80938551463965,1.,0.762546129463938));
#27322=CARTESIAN_POINT('Ctrl Pts',(-1.80351583877342,-1.,0.761915336443547));
#27323=CARTESIAN_POINT('Ctrl Pts',(-1.80351583877342,1.,0.761915336443547));
#27324=CARTESIAN_POINT('Ctrl Pts',(-1.79768986997783,-1.,0.761229695230558));
#27325=CARTESIAN_POINT('Ctrl Pts',(-1.79768986997783,1.,0.761229695230558));
#27326=CARTESIAN_POINT('Ctrl Pts',(-1.7918581561088,-1.,0.760469555880749));
#27327=CARTESIAN_POINT('Ctrl Pts',(-1.7918581561088,1.,0.760469555880749));
#27328=CARTESIAN_POINT('Ctrl Pts',(-1.78596964884604,-1.,0.759614401110189));
#27329=CARTESIAN_POINT('Ctrl Pts',(-1.78596964884604,1.,0.759614401110189));
#27330=CARTESIAN_POINT('Ctrl Pts',(-1.77999411220945,-1.,0.758650626677518));
#27331=CARTESIAN_POINT('Ctrl Pts',(-1.77999411220945,1.,0.758650626677518));
#27332=CARTESIAN_POINT('Ctrl Pts',(-1.77394167108292,-1.,0.757578264077029));
#27333=CARTESIAN_POINT('Ctrl Pts',(-1.77394167108292,1.,0.757578264077029));
#27334=CARTESIAN_POINT('Ctrl Pts',(-1.76789396002998,-1.,0.75642189602781));
#27335=CARTESIAN_POINT('Ctrl Pts',(-1.76789396002998,1.,0.75642189602781));
#27336=CARTESIAN_POINT('Ctrl Pts',(-1.76197817240128,-1.,0.755220979974461));
#27337=CARTESIAN_POINT('Ctrl Pts',(-1.76197817240128,1.,0.755220979974461));
#27338=CARTESIAN_POINT('Ctrl Pts',(-1.75631083600019,-1.,0.754009254027829));
#27339=CARTESIAN_POINT('Ctrl Pts',(-1.75631083600019,1.,0.754009254027829));
#27340=CARTESIAN_POINT('Ctrl Pts',(-1.75095139468794,-1.,0.752797683531314));
#27341=CARTESIAN_POINT('Ctrl Pts',(-1.75095139468794,1.,0.752797683531314));
#27342=CARTESIAN_POINT('Ctrl Pts',(-1.74585086852502,-1.,0.751555614164482));
#27343=CARTESIAN_POINT('Ctrl Pts',(-1.74585086852502,1.,0.751555614164482));
#27344=CARTESIAN_POINT('Ctrl Pts',(-1.74080458267114,-1.,0.750193435981249));
#27345=CARTESIAN_POINT('Ctrl Pts',(-1.74080458267114,1.,0.750193435981249));
#27346=CARTESIAN_POINT('Ctrl Pts',(-1.7355035168033,-1.,0.74858246295687));
#27347=CARTESIAN_POINT('Ctrl Pts',(-1.7355035168033,1.,0.74858246295687));
#27348=CARTESIAN_POINT('Ctrl Pts',(-1.72958533647714,-1.,0.746574710097752));
#27349=CARTESIAN_POINT('Ctrl Pts',(-1.72958533647714,1.,0.746574710097752));
#27350=CARTESIAN_POINT('Ctrl Pts',(-1.72268229916769,-1.,0.744021445433093));
#27351=CARTESIAN_POINT('Ctrl Pts',(-1.72268229916769,1.,0.744021445433093));
#27352=CARTESIAN_POINT('Ctrl Pts',(-1.71447789751001,-1.,0.74079516202821));
#27353=CARTESIAN_POINT('Ctrl Pts',(-1.71447789751001,1.,0.74079516202821));
#27354=CARTESIAN_POINT('Ctrl Pts',(-1.70473309004249,-1.,0.736799665716932));
#27355=CARTESIAN_POINT('Ctrl Pts',(-1.70473309004249,1.,0.736799665716932));
#27356=CARTESIAN_POINT('Ctrl Pts',(-1.69326921972915,-1.,0.731963238685357));
#27357=CARTESIAN_POINT('Ctrl Pts',(-1.69326921972915,1.,0.731963238685357));
#27358=CARTESIAN_POINT('Ctrl Pts',(-1.67996158451922,-1.,0.726235967982445));
#27359=CARTESIAN_POINT('Ctrl Pts',(-1.67996158451922,1.,0.726235967982445));
#27360=CARTESIAN_POINT('Ctrl Pts',(-1.66472880551777,-1.,0.71958543378795));
#27361=CARTESIAN_POINT('Ctrl Pts',(-1.66472880551777,1.,0.71958543378795));
#27362=CARTESIAN_POINT('Ctrl Pts',(-1.64752408828442,-1.,0.711993139340447));
#27363=CARTESIAN_POINT('Ctrl Pts',(-1.64752408828442,1.,0.711993139340447));
#27364=CARTESIAN_POINT('Ctrl Pts',(-1.6321654166204,-1.,0.705159151977294));
#27365=CARTESIAN_POINT('Ctrl Pts',(-1.6321654166204,1.,0.705159151977294));
#27366=CARTESIAN_POINT('Ctrl Pts',(-1.61974673471117,-1.,0.699605146398837));
#27367=CARTESIAN_POINT('Ctrl Pts',(-1.61974673471117,1.,0.699605146398837));
#27368=CARTESIAN_POINT('Ctrl Pts',(-1.61106790957619,-1.,0.69571209787897));
#27369=CARTESIAN_POINT('Ctrl Pts',(-1.61106790957619,1.,0.69571209787897));
#27370=CARTESIAN_POINT('Ctrl Pts',(-1.60662857109684,-1.,0.693717979106305));
#27371=CARTESIAN_POINT('Ctrl Pts',(-1.60662857109684,1.,0.693717979106305));
#27372=CARTESIAN_POINT('',(-2.0698113262342,1.,0.7455743247944));
#27373=CARTESIAN_POINT('Ctrl Pts',(-2.0698113262342,1.,0.7455743247944));
#27374=CARTESIAN_POINT('Ctrl Pts',(-2.06854248895728,1.,0.745832791378367));
#27375=CARTESIAN_POINT('Ctrl Pts',(-2.06600523016815,1.,0.7463458715442));
#27376=CARTESIAN_POINT('Ctrl Pts',(-2.06220058927826,1.,0.747103932787919));
#27377=CARTESIAN_POINT('Ctrl Pts',(-2.05713023031006,1.,0.748091554183802));
#27378=CARTESIAN_POINT('Ctrl Pts',(-2.05079645592154,1.,0.749287468665046));
#27379=CARTESIAN_POINT('Ctrl Pts',(-2.04446689147979,1.,0.750444657875576));
#27380=CARTESIAN_POINT('Ctrl Pts',(-2.03814160092099,1.,0.751562963361115));
#27381=CARTESIAN_POINT('Ctrl Pts',(-2.03182068456221,1.,0.752642180487211));
#27382=CARTESIAN_POINT('Ctrl Pts',(-2.02550428623313,1.,0.753682061112768));
#27383=CARTESIAN_POINT('Ctrl Pts',(-2.01919259405809,1.,0.754682330722816));
#27384=CARTESIAN_POINT('Ctrl Pts',(-2.01288584328084,1.,0.755642704957865));
#27385=CARTESIAN_POINT('Ctrl Pts',(-2.0065843158773,1.,0.75656290464667));
#27386=CARTESIAN_POINT('Ctrl Pts',(-2.00028834739178,1.,0.757442676862724));
#27387=CARTESIAN_POINT('Ctrl Pts',(-1.99399831098817,1.,0.758281796766761));
#27388=CARTESIAN_POINT('Ctrl Pts',(-1.98771456680874,1.,0.759080037802488));
#27389=CARTESIAN_POINT('Ctrl Pts',(-1.98143741418172,1.,0.75983714745219));
#27390=CARTESIAN_POINT('Ctrl Pts',(-1.97516705321494,1.,0.760552825409757));
#27391=CARTESIAN_POINT('Ctrl Pts',(-1.96890351582499,1.,0.76122669048382));
#27392=CARTESIAN_POINT('Ctrl Pts',(-1.96264672744186,1.,0.761858300014423));
#27393=CARTESIAN_POINT('Ctrl Pts',(-1.95639665309869,1.,0.762447203806179));
#27394=CARTESIAN_POINT('Ctrl Pts',(-1.95015342590024,1.,0.762992990878769));
#27395=CARTESIAN_POINT('Ctrl Pts',(-1.9439174661764,1.,0.763495333538629));
#27396=CARTESIAN_POINT('Ctrl Pts',(-1.93768964875886,1.,0.763954049121458));
#27397=CARTESIAN_POINT('Ctrl Pts',(-1.93147105496382,1.,0.76436901067394));
#27398=CARTESIAN_POINT('Ctrl Pts',(-1.92526263537048,1.,0.764740025488211));
#27399=CARTESIAN_POINT('Ctrl Pts',(-1.91906491634196,1.,0.765066729667088));
#27400=CARTESIAN_POINT('Ctrl Pts',(-1.91287765805169,1.,0.765348465884722));
#27401=CARTESIAN_POINT('Ctrl Pts',(-1.90669961402356,1.,0.765584196937919));
#27402=CARTESIAN_POINT('Ctrl Pts',(-1.90052930393596,1.,0.765772772593386));
#27403=CARTESIAN_POINT('Ctrl Pts',(-1.89436577771388,1.,0.765913193856978));
#27404=CARTESIAN_POINT('Ctrl Pts',(-1.88820926433409,1.,0.766004837062091));
#27405=CARTESIAN_POINT('Ctrl Pts',(-1.88206215302561,1.,0.766047794851864));
#27406=CARTESIAN_POINT('Ctrl Pts',(-1.87592888967883,1.,0.766042837036744));
#27407=CARTESIAN_POINT('Ctrl Pts',(-1.86981398314341,1.,0.765990708546091));
#27408=CARTESIAN_POINT('Ctrl Pts',(-1.86372027063312,1.,0.765891519092547));
#27409=CARTESIAN_POINT('Ctrl Pts',(-1.85764741390394,1.,0.765744212909318));
#27410=CARTESIAN_POINT('Ctrl Pts',(-1.85158945130063,1.,0.765545710619062));
#27411=CARTESIAN_POINT('Ctrl Pts',(-1.84553698875924,1.,0.765291664862029));
#27412=CARTESIAN_POINT('Ctrl Pts',(-1.83948181064835,1.,0.764978057881737));
#27413=CARTESIAN_POINT('Ctrl Pts',(-1.83342077227142,1.,0.764602549687853));
#27414=CARTESIAN_POINT('Ctrl Pts',(-1.82735991200065,1.,0.764165902605995));
#27415=CARTESIAN_POINT('Ctrl Pts',(-1.82131873145266,1.,0.763673465462726));
#27416=CARTESIAN_POINT('Ctrl Pts',(-1.8153211840553,1.,0.763132003836634));
#27417=CARTESIAN_POINT('Ctrl Pts',(-1.80938551463965,1.,0.762546129463938));
#27418=CARTESIAN_POINT('Ctrl Pts',(-1.80351583877342,1.,0.761915336443547));
#27419=CARTESIAN_POINT('Ctrl Pts',(-1.79768986997783,1.,0.761229695230558));
#27420=CARTESIAN_POINT('Ctrl Pts',(-1.7918581561088,1.,0.760469555880749));
#27421=CARTESIAN_POINT('Ctrl Pts',(-1.78596964884604,1.,0.759614401110189));
#27422=CARTESIAN_POINT('Ctrl Pts',(-1.77999411220945,1.,0.758650626677518));
#27423=CARTESIAN_POINT('Ctrl Pts',(-1.77394167108292,1.,0.757578264077029));
#27424=CARTESIAN_POINT('Ctrl Pts',(-1.76789396002998,1.,0.75642189602781));
#27425=CARTESIAN_POINT('Ctrl Pts',(-1.76197817240128,1.,0.755220979974461));
#27426=CARTESIAN_POINT('Ctrl Pts',(-1.75631083600019,1.,0.754009254027829));
#27427=CARTESIAN_POINT('Ctrl Pts',(-1.75095139468794,1.,0.752797683531314));
#27428=CARTESIAN_POINT('Ctrl Pts',(-1.74585086852502,1.,0.751555614164482));
#27429=CARTESIAN_POINT('Ctrl Pts',(-1.74080458267114,1.,0.750193435981249));
#27430=CARTESIAN_POINT('Ctrl Pts',(-1.7355035168033,1.,0.74858246295687));
#27431=CARTESIAN_POINT('Ctrl Pts',(-1.72958533647714,1.,0.746574710097752));
#27432=CARTESIAN_POINT('Ctrl Pts',(-1.72268229916769,1.,0.744021445433093));
#27433=CARTESIAN_POINT('Ctrl Pts',(-1.71447789751001,1.,0.74079516202821));
#27434=CARTESIAN_POINT('Ctrl Pts',(-1.70473309004249,1.,0.736799665716932));
#27435=CARTESIAN_POINT('Ctrl Pts',(-1.69326921972915,1.,0.731963238685357));
#27436=CARTESIAN_POINT('Ctrl Pts',(-1.67996158451922,1.,0.726235967982445));
#27437=CARTESIAN_POINT('Ctrl Pts',(-1.66472880551777,1.,0.71958543378795));
#27438=CARTESIAN_POINT('Ctrl Pts',(-1.64752408828442,1.,0.711993139340447));
#27439=CARTESIAN_POINT('Ctrl Pts',(-1.6321654166204,1.,0.705159151977294));
#27440=CARTESIAN_POINT('Ctrl Pts',(-1.61974673471117,1.,0.699605146398837));
#27441=CARTESIAN_POINT('Ctrl Pts',(-1.61106790957619,1.,0.69571209787897));
#27442=CARTESIAN_POINT('Ctrl Pts',(-1.60662857109684,1.,0.693717979106305));
#27443=CARTESIAN_POINT('',(-2.0698113262342,0.,0.7455743247944));
#27444=CARTESIAN_POINT('Origin',(-2.11275013067528,0.,0.61342227326009));
#27445=CARTESIAN_POINT('',(-2.11275013067528,1.,0.61342227326009));
#27446=CARTESIAN_POINT('',(-2.0698113262342,1.,0.7455743247944));
#27447=CARTESIAN_POINT('',(-2.11275013067528,0.,0.61342227326009));
#27448=CARTESIAN_POINT('Ctrl Pts',(-1.7075470150345,-1.,0.383122945602004));
#27449=CARTESIAN_POINT('Ctrl Pts',(-1.7075470150345,1.,0.383122945602004));
#27450=CARTESIAN_POINT('Ctrl Pts',(-1.71231062891958,-1.,0.384119047315542));
#27451=CARTESIAN_POINT('Ctrl Pts',(-1.71231062891958,1.,0.384119047315542));
#27452=CARTESIAN_POINT('Ctrl Pts',(-1.72162022246158,-1.,0.38607079032701));
#27453=CARTESIAN_POINT('Ctrl Pts',(-1.72162022246158,1.,0.38607079032701));
#27454=CARTESIAN_POINT('Ctrl Pts',(-1.7349317097561,-1.,0.388877023509191));
#27455=CARTESIAN_POINT('Ctrl Pts',(-1.7349317097561,1.,0.388877023509191));
#27456=CARTESIAN_POINT('Ctrl Pts',(-1.75137405313962,-1.,0.392375812294307));
#27457=CARTESIAN_POINT('Ctrl Pts',(-1.75137405313962,1.,0.392375812294307));
#27458=CARTESIAN_POINT('Ctrl Pts',(-1.7697556004756,-1.,0.39634619612042));
#27459=CARTESIAN_POINT('Ctrl Pts',(-1.7697556004756,1.,0.39634619612042));
#27460=CARTESIAN_POINT('Ctrl Pts',(-1.78598826347533,-1.,0.39991940378308));
#27461=CARTESIAN_POINT('Ctrl Pts',(-1.78598826347533,1.,0.39991940378308));
#27462=CARTESIAN_POINT('Ctrl Pts',(-1.80012077176221,-1.,0.403107976170441));
#27463=CARTESIAN_POINT('Ctrl Pts',(-1.80012077176221,1.,0.403107976170441));
#27464=CARTESIAN_POINT('Ctrl Pts',(-1.81223801813988,-1.,0.405933518411838));
#27465=CARTESIAN_POINT('Ctrl Pts',(-1.81223801813988,1.,0.405933518411838));
#27466=CARTESIAN_POINT('Ctrl Pts',(-1.8224702267854,-1.,0.408428948108533));
#27467=CARTESIAN_POINT('Ctrl Pts',(-1.8224702267854,1.,0.408428948108533));
#27468=CARTESIAN_POINT('Ctrl Pts',(-1.83100408895216,-1.,0.410641256301675));
#27469=CARTESIAN_POINT('Ctrl Pts',(-1.83100408895216,1.,0.410641256301675));
#27470=CARTESIAN_POINT('Ctrl Pts',(-1.83808953475839,-1.,0.412633125322161));
#27471=CARTESIAN_POINT('Ctrl Pts',(-1.83808953475839,1.,0.412633125322161));
#27472=CARTESIAN_POINT('Ctrl Pts',(-1.8440575707371,-1.,0.41448743825434));
#27473=CARTESIAN_POINT('Ctrl Pts',(-1.8440575707371,1.,0.41448743825434));
#27474=CARTESIAN_POINT('Ctrl Pts',(-1.84929312929882,-1.,0.416300022038864));
#27475=CARTESIAN_POINT('Ctrl Pts',(-1.84929312929882,1.,0.416300022038864));
#27476=CARTESIAN_POINT('Ctrl Pts',(-1.85417632856234,-1.,0.418164129143534));
#27477=CARTESIAN_POINT('Ctrl Pts',(-1.85417632856234,1.,0.418164129143534));
#27478=CARTESIAN_POINT('Ctrl Pts',(-1.85903281096686,-1.,0.420157287975619));
#27479=CARTESIAN_POINT('Ctrl Pts',(-1.85903281096686,1.,0.420157287975619));
#27480=CARTESIAN_POINT('Ctrl Pts',(-1.86408083334028,-1.,0.422327307418275));
#27481=CARTESIAN_POINT('Ctrl Pts',(-1.86408083334028,1.,0.422327307418275));
#27482=CARTESIAN_POINT('Ctrl Pts',(-1.86937803944323,-1.,0.424678177291359));
#27483=CARTESIAN_POINT('Ctrl Pts',(-1.86937803944323,1.,0.424678177291359));
#27484=CARTESIAN_POINT('Ctrl Pts',(-1.87486989291484,-1.,0.427183828519102));
#27485=CARTESIAN_POINT('Ctrl Pts',(-1.87486989291484,1.,0.427183828519102));
#27486=CARTESIAN_POINT('Ctrl Pts',(-1.88044229001832,-1.,0.429803062482344));
#27487=CARTESIAN_POINT('Ctrl Pts',(-1.88044229001832,1.,0.429803062482344));
#27488=CARTESIAN_POINT('Ctrl Pts',(-1.88596913666793,-1.,0.432493038548748));
#27489=CARTESIAN_POINT('Ctrl Pts',(-1.88596913666793,1.,0.432493038548748));
#27490=CARTESIAN_POINT('Ctrl Pts',(-1.89136993975504,-1.,0.435225660963383));
#27491=CARTESIAN_POINT('Ctrl Pts',(-1.89136993975504,1.,0.435225660963383));
#27492=CARTESIAN_POINT('Ctrl Pts',(-1.89663648956466,-1.,0.437995003948244));
#27493=CARTESIAN_POINT('Ctrl Pts',(-1.89663648956466,1.,0.437995003948244));
#27494=CARTESIAN_POINT('Ctrl Pts',(-1.90180124389086,-1.,0.440807833704038));
#27495=CARTESIAN_POINT('Ctrl Pts',(-1.90180124389086,1.,0.440807833704038));
#27496=CARTESIAN_POINT('Ctrl Pts',(-1.90691756144898,-1.,0.44367755684915));
#27497=CARTESIAN_POINT('Ctrl Pts',(-1.90691756144898,1.,0.44367755684915));
#27498=CARTESIAN_POINT('Ctrl Pts',(-1.9120369998112,-1.,0.446617343485711));
#27499=CARTESIAN_POINT('Ctrl Pts',(-1.9120369998112,1.,0.446617343485711));
#27500=CARTESIAN_POINT('Ctrl Pts',(-1.91718342555755,-1.,0.449632260106662));
#27501=CARTESIAN_POINT('Ctrl Pts',(-1.91718342555755,1.,0.449632260106662));
#27502=CARTESIAN_POINT('Ctrl Pts',(-1.92235380648502,-1.,0.452719478359432));
#27503=CARTESIAN_POINT('Ctrl Pts',(-1.92235380648502,1.,0.452719478359432));
#27504=CARTESIAN_POINT('Ctrl Pts',(-1.92753067150476,-1.,0.455872005174371));
#27505=CARTESIAN_POINT('Ctrl Pts',(-1.92753067150476,1.,0.455872005174371));
#27506=CARTESIAN_POINT('Ctrl Pts',(-1.93269066517934,-1.,0.459081234547926));
#27507=CARTESIAN_POINT('Ctrl Pts',(-1.93269066517934,1.,0.459081234547926));
#27508=CARTESIAN_POINT('Ctrl Pts',(-1.93781486640821,-1.,0.462340031009056));
#27509=CARTESIAN_POINT('Ctrl Pts',(-1.93781486640821,1.,0.462340031009056));
#27510=CARTESIAN_POINT('Ctrl Pts',(-1.9428979419619,-1.,0.46564546202603));
#27511=CARTESIAN_POINT('Ctrl Pts',(-1.9428979419619,1.,0.46564546202603));
#27512=CARTESIAN_POINT('Ctrl Pts',(-1.94794381136514,-1.,0.468997482913135));
#27513=CARTESIAN_POINT('Ctrl Pts',(-1.94794381136514,1.,0.468997482913135));
#27514=CARTESIAN_POINT('Ctrl Pts',(-1.95296148278133,-1.,0.472397672264072));
#27515=CARTESIAN_POINT('Ctrl Pts',(-1.95296148278133,1.,0.472397672264072));
#27516=CARTESIAN_POINT('Ctrl Pts',(-1.95796111148177,-1.,0.475848034683176));
#27517=CARTESIAN_POINT('Ctrl Pts',(-1.95796111148177,1.,0.475848034683176));
#27518=CARTESIAN_POINT('Ctrl Pts',(-1.96294933055943,-1.,0.479349583074855));
#27519=CARTESIAN_POINT('Ctrl Pts',(-1.96294933055943,1.,0.479349583074855));
#27520=CARTESIAN_POINT('Ctrl Pts',(-1.96792703422362,-1.,0.48290166212069));
#27521=CARTESIAN_POINT('Ctrl Pts',(-1.96792703422362,1.,0.48290166212069));
#27522=CARTESIAN_POINT('Ctrl Pts',(-1.97289186263272,-1.,0.486502692907659));
#27523=CARTESIAN_POINT('Ctrl Pts',(-1.97289186263272,1.,0.486502692907659));
#27524=CARTESIAN_POINT('Ctrl Pts',(-1.97783973019229,-1.,0.490150627860952));
#27525=CARTESIAN_POINT('Ctrl Pts',(-1.97783973019229,1.,0.490150627860952));
#27526=CARTESIAN_POINT('Ctrl Pts',(-1.98276658761821,-1.,0.493843476541494));
#27527=CARTESIAN_POINT('Ctrl Pts',(-1.98276658761821,1.,0.493843476541494));
#27528=CARTESIAN_POINT('Ctrl Pts',(-1.98767044752932,-1.,0.497579909545574));
#27529=CARTESIAN_POINT('Ctrl Pts',(-1.98767044752932,1.,0.497579909545574));
#27530=CARTESIAN_POINT('Ctrl Pts',(-1.99255149126155,-1.,0.501359287727146));
#27531=CARTESIAN_POINT('Ctrl Pts',(-1.99255149126155,1.,0.501359287727146));
#27532=CARTESIAN_POINT('Ctrl Pts',(-1.99741107463572,-1.,0.505181361323026));
#27533=CARTESIAN_POINT('Ctrl Pts',(-1.99741107463572,1.,0.505181361323026));
#27534=CARTESIAN_POINT('Ctrl Pts',(-2.00225107134734,-1.,0.509046069886157));
#27535=CARTESIAN_POINT('Ctrl Pts',(-2.00225107134734,1.,0.509046069886157));
#27536=CARTESIAN_POINT('Ctrl Pts',(-2.00707309946949,-1.,0.512953306961792));
#27537=CARTESIAN_POINT('Ctrl Pts',(-2.00707309946949,1.,0.512953306961792));
#27538=CARTESIAN_POINT('Ctrl Pts',(-2.01187773939242,-1.,0.516902681728687));
#27539=CARTESIAN_POINT('Ctrl Pts',(-2.01187773939242,1.,0.516902681728687));
#27540=CARTESIAN_POINT('Ctrl Pts',(-2.01666477917286,-1.,0.52089359039937));
#27541=CARTESIAN_POINT('Ctrl Pts',(-2.01666477917286,1.,0.52089359039937));
#27542=CARTESIAN_POINT('Ctrl Pts',(-2.02143356304698,-1.,0.524925318333476));
#27543=CARTESIAN_POINT('Ctrl Pts',(-2.02143356304698,1.,0.524925318333476));
#27544=CARTESIAN_POINT('Ctrl Pts',(-2.0261832908329,-1.,0.528997127241914));
#27545=CARTESIAN_POINT('Ctrl Pts',(-2.0261832908329,1.,0.528997127241914));
#27546=CARTESIAN_POINT('Ctrl Pts',(-2.03091336214426,-1.,0.533108355132976));
#27547=CARTESIAN_POINT('Ctrl Pts',(-2.03091336214426,1.,0.533108355132976));
#27548=CARTESIAN_POINT('Ctrl Pts',(-2.03562362954037,-1.,0.537258489833262));
#27549=CARTESIAN_POINT('Ctrl Pts',(-2.03562362954037,1.,0.537258489833262));
#27550=CARTESIAN_POINT('Ctrl Pts',(-2.04031422690527,-1.,0.541447120615659));
#27551=CARTESIAN_POINT('Ctrl Pts',(-2.04031422690527,1.,0.541447120615659));
#27552=CARTESIAN_POINT('Ctrl Pts',(-2.04498544714588,-1.,0.54567390381743));
#27553=CARTESIAN_POINT('Ctrl Pts',(-2.04498544714588,1.,0.54567390381743));
#27554=CARTESIAN_POINT('Ctrl Pts',(-2.04963761077958,-1.,0.549938525150295));
#27555=CARTESIAN_POINT('Ctrl Pts',(-2.04963761077958,1.,0.549938525150295));
#27556=CARTESIAN_POINT('Ctrl Pts',(-2.05427091604413,-1.,0.554240657463906));
#27557=CARTESIAN_POINT('Ctrl Pts',(-2.05427091604413,1.,0.554240657463906));
#27558=CARTESIAN_POINT('Ctrl Pts',(-2.05888537756462,-1.,0.558579940185151));
#27559=CARTESIAN_POINT('Ctrl Pts',(-2.05888537756462,1.,0.558579940185151));
#27560=CARTESIAN_POINT('Ctrl Pts',(-2.06348090160589,-1.,0.562955993082261));
#27561=CARTESIAN_POINT('Ctrl Pts',(-2.06348090160589,1.,0.562955993082261));
#27562=CARTESIAN_POINT('Ctrl Pts',(-2.06805732997334,-1.,0.567368421181087));
#27563=CARTESIAN_POINT('Ctrl Pts',(-2.06805732997334,1.,0.567368421181087));
#27564=CARTESIAN_POINT('Ctrl Pts',(-2.07261449292824,-1.,0.571816823242603));
#27565=CARTESIAN_POINT('Ctrl Pts',(-2.07261449292824,1.,0.571816823242603));
#27566=CARTESIAN_POINT('Ctrl Pts',(-2.07715226767559,-1.,0.576300797416844));
#27567=CARTESIAN_POINT('Ctrl Pts',(-2.07715226767559,1.,0.576300797416844));
#27568=CARTESIAN_POINT('Ctrl Pts',(-2.08167059018418,-1.,0.580819952108063));
#27569=CARTESIAN_POINT('Ctrl Pts',(-2.08167059018418,1.,0.580819952108063));
#27570=CARTESIAN_POINT('Ctrl Pts',(-2.08616943727951,-1.,0.585373918991617));
#27571=CARTESIAN_POINT('Ctrl Pts',(-2.08616943727951,1.,0.585373918991617));
#27572=CARTESIAN_POINT('Ctrl Pts',(-2.09064881812129,-1.,0.589962365403406));
#27573=CARTESIAN_POINT('Ctrl Pts',(-2.09064881812129,1.,0.589962365403406));
#27574=CARTESIAN_POINT('Ctrl Pts',(-2.0951087622027,-1.,0.594585006052162));
#27575=CARTESIAN_POINT('Ctrl Pts',(-2.0951087622027,1.,0.594585006052162));
#27576=CARTESIAN_POINT('Ctrl Pts',(-2.0995493086477,-1.,0.599241616420533));
#27577=CARTESIAN_POINT('Ctrl Pts',(-2.0995493086477,1.,0.599241616420533));
#27578=CARTESIAN_POINT('Ctrl Pts',(-2.10397049886949,-1.,0.60393203073603));
#27579=CARTESIAN_POINT('Ctrl Pts',(-2.10397049886949,1.,0.60393203073603));
#27580=CARTESIAN_POINT('Ctrl Pts',(-2.1074919961518,-1.,0.607711315454876));
#27581=CARTESIAN_POINT('Ctrl Pts',(-2.1074919961518,1.,0.607711315454876));
#27582=CARTESIAN_POINT('Ctrl Pts',(-2.11012443807238,-1.,0.610560911689899));
#27583=CARTESIAN_POINT('Ctrl Pts',(-2.11012443807238,1.,0.610560911689899));
#27584=CARTESIAN_POINT('Ctrl Pts',(-2.11187554259986,-1.,0.6124673655618));
#27585=CARTESIAN_POINT('Ctrl Pts',(-2.11187554259986,1.,0.6124673655618));
#27586=CARTESIAN_POINT('Ctrl Pts',(-2.11275013067528,-1.,0.61342227326009));
#27587=CARTESIAN_POINT('Ctrl Pts',(-2.11275013067528,1.,0.61342227326009));
#27588=CARTESIAN_POINT('',(-1.7075470150345,1.,0.383122945602004));
#27589=CARTESIAN_POINT('Ctrl Pts',(-1.7075470150345,1.,0.383122945602004));
#27590=CARTESIAN_POINT('Ctrl Pts',(-1.71231062891958,1.,0.384119047315542));
#27591=CARTESIAN_POINT('Ctrl Pts',(-1.72162022246158,1.,0.38607079032701));
#27592=CARTESIAN_POINT('Ctrl Pts',(-1.7349317097561,1.,0.388877023509191));
#27593=CARTESIAN_POINT('Ctrl Pts',(-1.75137405313962,1.,0.392375812294307));
#27594=CARTESIAN_POINT('Ctrl Pts',(-1.7697556004756,1.,0.39634619612042));
#27595=CARTESIAN_POINT('Ctrl Pts',(-1.78598826347533,1.,0.39991940378308));
#27596=CARTESIAN_POINT('Ctrl Pts',(-1.80012077176221,1.,0.403107976170441));
#27597=CARTESIAN_POINT('Ctrl Pts',(-1.81223801813988,1.,0.405933518411838));
#27598=CARTESIAN_POINT('Ctrl Pts',(-1.8224702267854,1.,0.408428948108533));
#27599=CARTESIAN_POINT('Ctrl Pts',(-1.83100408895216,1.,0.410641256301675));
#27600=CARTESIAN_POINT('Ctrl Pts',(-1.83808953475839,1.,0.412633125322161));
#27601=CARTESIAN_POINT('Ctrl Pts',(-1.8440575707371,1.,0.41448743825434));
#27602=CARTESIAN_POINT('Ctrl Pts',(-1.84929312929882,1.,0.416300022038864));
#27603=CARTESIAN_POINT('Ctrl Pts',(-1.85417632856234,1.,0.418164129143534));
#27604=CARTESIAN_POINT('Ctrl Pts',(-1.85903281096686,1.,0.420157287975619));
#27605=CARTESIAN_POINT('Ctrl Pts',(-1.86408083334028,1.,0.422327307418275));
#27606=CARTESIAN_POINT('Ctrl Pts',(-1.86937803944323,1.,0.424678177291359));
#27607=CARTESIAN_POINT('Ctrl Pts',(-1.87486989291484,1.,0.427183828519102));
#27608=CARTESIAN_POINT('Ctrl Pts',(-1.88044229001832,1.,0.429803062482344));
#27609=CARTESIAN_POINT('Ctrl Pts',(-1.88596913666793,1.,0.432493038548748));
#27610=CARTESIAN_POINT('Ctrl Pts',(-1.89136993975504,1.,0.435225660963383));
#27611=CARTESIAN_POINT('Ctrl Pts',(-1.89663648956466,1.,0.437995003948244));
#27612=CARTESIAN_POINT('Ctrl Pts',(-1.90180124389086,1.,0.440807833704038));
#27613=CARTESIAN_POINT('Ctrl Pts',(-1.90691756144898,1.,0.44367755684915));
#27614=CARTESIAN_POINT('Ctrl Pts',(-1.9120369998112,1.,0.446617343485711));
#27615=CARTESIAN_POINT('Ctrl Pts',(-1.91718342555755,1.,0.449632260106662));
#27616=CARTESIAN_POINT('Ctrl Pts',(-1.92235380648502,1.,0.452719478359432));
#27617=CARTESIAN_POINT('Ctrl Pts',(-1.92753067150476,1.,0.455872005174371));
#27618=CARTESIAN_POINT('Ctrl Pts',(-1.93269066517934,1.,0.459081234547926));
#27619=CARTESIAN_POINT('Ctrl Pts',(-1.93781486640821,1.,0.462340031009056));
#27620=CARTESIAN_POINT('Ctrl Pts',(-1.9428979419619,1.,0.46564546202603));
#27621=CARTESIAN_POINT('Ctrl Pts',(-1.94794381136514,1.,0.468997482913135));
#27622=CARTESIAN_POINT('Ctrl Pts',(-1.95296148278133,1.,0.472397672264072));
#27623=CARTESIAN_POINT('Ctrl Pts',(-1.95796111148177,1.,0.475848034683176));
#27624=CARTESIAN_POINT('Ctrl Pts',(-1.96294933055943,1.,0.479349583074855));
#27625=CARTESIAN_POINT('Ctrl Pts',(-1.96792703422362,1.,0.48290166212069));
#27626=CARTESIAN_POINT('Ctrl Pts',(-1.97289186263272,1.,0.486502692907659));
#27627=CARTESIAN_POINT('Ctrl Pts',(-1.97783973019229,1.,0.490150627860952));
#27628=CARTESIAN_POINT('Ctrl Pts',(-1.98276658761821,1.,0.493843476541494));
#27629=CARTESIAN_POINT('Ctrl Pts',(-1.98767044752932,1.,0.497579909545574));
#27630=CARTESIAN_POINT('Ctrl Pts',(-1.99255149126155,1.,0.501359287727146));
#27631=CARTESIAN_POINT('Ctrl Pts',(-1.99741107463572,1.,0.505181361323026));
#27632=CARTESIAN_POINT('Ctrl Pts',(-2.00225107134734,1.,0.509046069886157));
#27633=CARTESIAN_POINT('Ctrl Pts',(-2.00707309946949,1.,0.512953306961792));
#27634=CARTESIAN_POINT('Ctrl Pts',(-2.01187773939242,1.,0.516902681728687));
#27635=CARTESIAN_POINT('Ctrl Pts',(-2.01666477917286,1.,0.52089359039937));
#27636=CARTESIAN_POINT('Ctrl Pts',(-2.02143356304698,1.,0.524925318333476));
#27637=CARTESIAN_POINT('Ctrl Pts',(-2.0261832908329,1.,0.528997127241914));
#27638=CARTESIAN_POINT('Ctrl Pts',(-2.03091336214426,1.,0.533108355132976));
#27639=CARTESIAN_POINT('Ctrl Pts',(-2.03562362954037,1.,0.537258489833262));
#27640=CARTESIAN_POINT('Ctrl Pts',(-2.04031422690527,1.,0.541447120615659));
#27641=CARTESIAN_POINT('Ctrl Pts',(-2.04498544714588,1.,0.54567390381743));
#27642=CARTESIAN_POINT('Ctrl Pts',(-2.04963761077958,1.,0.549938525150295));
#27643=CARTESIAN_POINT('Ctrl Pts',(-2.05427091604413,1.,0.554240657463906));
#27644=CARTESIAN_POINT('Ctrl Pts',(-2.05888537756462,1.,0.558579940185151));
#27645=CARTESIAN_POINT('Ctrl Pts',(-2.06348090160589,1.,0.562955993082261));
#27646=CARTESIAN_POINT('Ctrl Pts',(-2.06805732997334,1.,0.567368421181087));
#27647=CARTESIAN_POINT('Ctrl Pts',(-2.07261449292824,1.,0.571816823242603));
#27648=CARTESIAN_POINT('Ctrl Pts',(-2.07715226767559,1.,0.576300797416844));
#27649=CARTESIAN_POINT('Ctrl Pts',(-2.08167059018418,1.,0.580819952108063));
#27650=CARTESIAN_POINT('Ctrl Pts',(-2.08616943727951,1.,0.585373918991617));
#27651=CARTESIAN_POINT('Ctrl Pts',(-2.09064881812129,1.,0.589962365403406));
#27652=CARTESIAN_POINT('Ctrl Pts',(-2.0951087622027,1.,0.594585006052162));
#27653=CARTESIAN_POINT('Ctrl Pts',(-2.0995493086477,1.,0.599241616420533));
#27654=CARTESIAN_POINT('Ctrl Pts',(-2.10397049886949,1.,0.60393203073603));
#27655=CARTESIAN_POINT('Ctrl Pts',(-2.1074919961518,1.,0.607711315454876));
#27656=CARTESIAN_POINT('Ctrl Pts',(-2.11012443807238,1.,0.610560911689899));
#27657=CARTESIAN_POINT('Ctrl Pts',(-2.11187554259986,1.,0.6124673655618));
#27658=CARTESIAN_POINT('Ctrl Pts',(-2.11275013067528,1.,0.61342227326009));
#27659=CARTESIAN_POINT('',(-1.7075470150345,0.,0.383122945602003));
#27660=CARTESIAN_POINT('Origin',(0.,0.,0.));
#27661=CARTESIAN_POINT('',(-1.74236521665491,1.,0.163289472382896));
#27662=CARTESIAN_POINT('Origin',(0.,1.,0.));
#27663=CARTESIAN_POINT('',(-1.74236521665491,0.,0.163289472382896));
#27664=CARTESIAN_POINT('Ctrl Pts',(-2.19890268624765,-1.,0.069476445021958));
#27665=CARTESIAN_POINT('Ctrl Pts',(-2.19890268624765,1.,0.069476445021958));
#27666=CARTESIAN_POINT('Ctrl Pts',(-2.19777582085423,-1.,0.0701143536325489));
#27667=CARTESIAN_POINT('Ctrl Pts',(-2.19777582085423,1.,0.0701143536325489));
#27668=CARTESIAN_POINT('Ctrl Pts',(-2.19552129484002,-1.,0.0713863779526153));
#27669=CARTESIAN_POINT('Ctrl Pts',(-2.19552129484002,1.,0.0713863779526153));
#27670=CARTESIAN_POINT('Ctrl Pts',(-2.19213712013662,-1.,0.0732830357306724));
#27671=CARTESIAN_POINT('Ctrl Pts',(-2.19213712013662,1.,0.0732830357306724));
#27672=CARTESIAN_POINT('Ctrl Pts',(-2.1876201139953,-1.,0.0757891465836146));
#27673=CARTESIAN_POINT('Ctrl Pts',(-2.1876201139953,1.,0.0757891465836146));
#27674=CARTESIAN_POINT('Ctrl Pts',(-2.18196589448887,-1.,0.0788837727685241));
#27675=CARTESIAN_POINT('Ctrl Pts',(-2.18196589448887,1.,0.0788837727685241));
#27676=CARTESIAN_POINT('Ctrl Pts',(-2.176303712113,-1.,0.0819402680872764));
#27677=CARTESIAN_POINT('Ctrl Pts',(-2.176303712113,1.,0.0819402680872764));
#27678=CARTESIAN_POINT('Ctrl Pts',(-2.17063357870952,-1.,0.0849584620835371));
#27679=CARTESIAN_POINT('Ctrl Pts',(-2.17063357870952,1.,0.0849584620835371));
#27680=CARTESIAN_POINT('Ctrl Pts',(-2.16495552645014,-1.,0.0879381291386921));
#27681=CARTESIAN_POINT('Ctrl Pts',(-2.16495552645014,1.,0.0879381291386921));
#27682=CARTESIAN_POINT('Ctrl Pts',(-2.15926961544516,-1.,0.0908789888107264));
#27683=CARTESIAN_POINT('Ctrl Pts',(-2.15926961544516,1.,0.0908789888107264));
#27684=CARTESIAN_POINT('Ctrl Pts',(-2.1535759397817,-1.,0.0937807218867642));
#27685=CARTESIAN_POINT('Ctrl Pts',(-2.1535759397817,1.,0.0937807218867642));
#27686=CARTESIAN_POINT('Ctrl Pts',(-2.14787463531795,-1.,0.0966429852305457));
#27687=CARTESIAN_POINT('Ctrl Pts',(-2.14787463531795,1.,0.0966429852305457));
#27688=CARTESIAN_POINT('Ctrl Pts',(-2.14216588396025,-1.,0.0994654261990914));
#27689=CARTESIAN_POINT('Ctrl Pts',(-2.14216588396025,1.,0.0994654261990914));
#27690=CARTESIAN_POINT('Ctrl Pts',(-2.13644992667165,-1.,0.1022477005561));
#27691=CARTESIAN_POINT('Ctrl Pts',(-2.13644992667165,1.,0.1022477005561));
#27692=CARTESIAN_POINT('Ctrl Pts',(-2.13072704887293,-1.,0.104989479152739));
#27693=CARTESIAN_POINT('Ctrl Pts',(-2.13072704887293,1.,0.104989479152739));
#27694=CARTESIAN_POINT('Ctrl Pts',(-2.12499752307,-1.,0.10769043523109));
#27695=CARTESIAN_POINT('Ctrl Pts',(-2.12499752307,1.,0.10769043523109));
#27696=CARTESIAN_POINT('Ctrl Pts',(-2.11926155590865,-1.,0.110350236135025));
#27697=CARTESIAN_POINT('Ctrl Pts',(-2.11926155590865,1.,0.110350236135025));
#27698=CARTESIAN_POINT('Ctrl Pts',(-2.11351924490306,-1.,0.112968534419737));
#27699=CARTESIAN_POINT('Ctrl Pts',(-2.11351924490306,1.,0.112968534419737));
#27700=CARTESIAN_POINT('Ctrl Pts',(-2.10777050261309,-1.,0.115544957687926));
#27701=CARTESIAN_POINT('Ctrl Pts',(-2.10777050261309,1.,0.115544957687926));
#27702=CARTESIAN_POINT('Ctrl Pts',(-2.102015121329,-1.,0.118079107988355));
#27703=CARTESIAN_POINT('Ctrl Pts',(-2.102015121329,1.,0.118079107988355));
#27704=CARTESIAN_POINT('Ctrl Pts',(-2.0962529286773,-1.,0.120570567965122));
#27705=CARTESIAN_POINT('Ctrl Pts',(-2.0962529286773,1.,0.120570567965122));
#27706=CARTESIAN_POINT('Ctrl Pts',(-2.09048392424825,-1.,0.123018905621083));
#27707=CARTESIAN_POINT('Ctrl Pts',(-2.09048392424825,1.,0.123018905621083));
#27708=CARTESIAN_POINT('Ctrl Pts',(-2.08470840653643,-1.,0.125423679412061));
#27709=CARTESIAN_POINT('Ctrl Pts',(-2.08470840653643,1.,0.125423679412061));
#27710=CARTESIAN_POINT('Ctrl Pts',(-2.07892715110987,-1.,0.12778444527612));
#27711=CARTESIAN_POINT('Ctrl Pts',(-2.07892715110987,1.,0.12778444527612));
#27712=CARTESIAN_POINT('Ctrl Pts',(-2.07314114713063,-1.,0.130100748328403));
#27713=CARTESIAN_POINT('Ctrl Pts',(-2.07314114713063,1.,0.130100748328403));
#27714=CARTESIAN_POINT('Ctrl Pts',(-2.06735123910326,-1.,0.13237211154771));
#27715=CARTESIAN_POINT('Ctrl Pts',(-2.06735123910326,1.,0.13237211154771));
#27716=CARTESIAN_POINT('Ctrl Pts',(-2.06155781517842,-1.,0.134598026192106));
#27717=CARTESIAN_POINT('Ctrl Pts',(-2.06155781517842,1.,0.134598026192106));
#27718=CARTESIAN_POINT('Ctrl Pts',(-2.05576044414264,-1.,0.136777941218043));
#27719=CARTESIAN_POINT('Ctrl Pts',(-2.05576044414264,1.,0.136777941218043));
#27720=CARTESIAN_POINT('Ctrl Pts',(-2.04995762001328,-1.,0.138911255368966));
#27721=CARTESIAN_POINT('Ctrl Pts',(-2.04995762001328,1.,0.138911255368966));
#27722=CARTESIAN_POINT('Ctrl Pts',(-2.04414757947916,-1.,0.140997332152546));
#27723=CARTESIAN_POINT('Ctrl Pts',(-2.04414757947916,1.,0.140997332152546));
#27724=CARTESIAN_POINT('Ctrl Pts',(-2.03832911025912,-1.,0.143035515058209));
#27725=CARTESIAN_POINT('Ctrl Pts',(-2.03832911025912,1.,0.143035515058209));
#27726=CARTESIAN_POINT('Ctrl Pts',(-2.03250223739942,-1.,0.145025140186057));
#27727=CARTESIAN_POINT('Ctrl Pts',(-2.03250223739942,1.,0.145025140186057));
#27728=CARTESIAN_POINT('Ctrl Pts',(-2.02666926182017,-1.,0.146965557332583));
#27729=CARTESIAN_POINT('Ctrl Pts',(-2.02666926182017,1.,0.146965557332583));
#27730=CARTESIAN_POINT('Ctrl Pts',(-2.02083464969894,-1.,0.148856124775337));
#27731=CARTESIAN_POINT('Ctrl Pts',(-2.02083464969894,1.,0.148856124775337));
#27732=CARTESIAN_POINT('Ctrl Pts',(-2.01500291940238,-1.,0.150696157673078));
#27733=CARTESIAN_POINT('Ctrl Pts',(-2.01500291940238,1.,0.150696157673078));
#27734=CARTESIAN_POINT('Ctrl Pts',(-2.00917680318424,-1.,0.15248488362145));
#27735=CARTESIAN_POINT('Ctrl Pts',(-2.00917680318424,1.,0.15248488362145));
#27736=CARTESIAN_POINT('Ctrl Pts',(-2.00335565310543,-1.,0.154221403049722));
#27737=CARTESIAN_POINT('Ctrl Pts',(-2.00335565310543,1.,0.154221403049722));
#27738=CARTESIAN_POINT('Ctrl Pts',(-1.99753284771497,-1.,0.155904629548783));
#27739=CARTESIAN_POINT('Ctrl Pts',(-1.99753284771497,1.,0.155904629548783));
#27740=CARTESIAN_POINT('Ctrl Pts',(-1.99169810931908,-1.,0.157533331459227));
#27741=CARTESIAN_POINT('Ctrl Pts',(-1.99169810931908,1.,0.157533331459227));
#27742=CARTESIAN_POINT('Ctrl Pts',(-1.98584238283292,-1.,0.159106226437299));
#27743=CARTESIAN_POINT('Ctrl Pts',(-1.98584238283292,1.,0.159106226437299));
#27744=CARTESIAN_POINT('Ctrl Pts',(-1.97996195437559,-1.,0.160622060784611));
#27745=CARTESIAN_POINT('Ctrl Pts',(-1.97996195437559,1.,0.160622060784611));
#27746=CARTESIAN_POINT('Ctrl Pts',(-1.97406280235188,-1.,0.162079693556288));
#27747=CARTESIAN_POINT('Ctrl Pts',(-1.97406280235188,1.,0.162079693556288));
#27748=CARTESIAN_POINT('Ctrl Pts',(-1.96816512677967,-1.,0.163478185457734));
#27749=CARTESIAN_POINT('Ctrl Pts',(-1.96816512677967,1.,0.163478185457734));
#27750=CARTESIAN_POINT('Ctrl Pts',(-1.96229379940136,-1.,0.164816568920269));
#27751=CARTESIAN_POINT('Ctrl Pts',(-1.96229379940136,1.,0.164816568920269));
#27752=CARTESIAN_POINT('Ctrl Pts',(-1.9564675971873,-1.,0.166093592002812));
#27753=CARTESIAN_POINT('Ctrl Pts',(-1.9564675971873,1.,0.166093592002812));
#27754=CARTESIAN_POINT('Ctrl Pts',(-1.95069027794294,-1.,0.167307501784475));
#27755=CARTESIAN_POINT('Ctrl Pts',(-1.95069027794294,1.,0.167307501784475));
#27756=CARTESIAN_POINT('Ctrl Pts',(-1.94493757756931,-1.,0.168455741607556));
#27757=CARTESIAN_POINT('Ctrl Pts',(-1.94493757756931,1.,0.168455741607556));
#27758=CARTESIAN_POINT('Ctrl Pts',(-1.93915639211581,-1.,0.169534904817491));
#27759=CARTESIAN_POINT('Ctrl Pts',(-1.93915639211581,1.,0.169534904817491));
#27760=CARTESIAN_POINT('Ctrl Pts',(-1.93329183155539,-1.,0.170541253116201));
#27761=CARTESIAN_POINT('Ctrl Pts',(-1.93329183155539,1.,0.170541253116201));
#27762=CARTESIAN_POINT('Ctrl Pts',(-1.92731093582036,-1.,0.171471191532988));
#27763=CARTESIAN_POINT('Ctrl Pts',(-1.92731093582036,1.,0.171471191532988));
#27764=CARTESIAN_POINT('Ctrl Pts',(-1.9212233439798,-1.,0.172321621259514));
#27765=CARTESIAN_POINT('Ctrl Pts',(-1.9212233439798,1.,0.172321621259514));
#27766=CARTESIAN_POINT('Ctrl Pts',(-1.91511429159527,-1.,0.173090695383496));
#27767=CARTESIAN_POINT('Ctrl Pts',(-1.91511429159527,1.,0.173090695383496));
#27768=CARTESIAN_POINT('Ctrl Pts',(-1.90911693975267,-1.,0.173776635257817));
#27769=CARTESIAN_POINT('Ctrl Pts',(-1.90911693975267,1.,0.173776635257817));
#27770=CARTESIAN_POINT('Ctrl Pts',(-1.90335253862834,-1.,0.174375518661085));
#27771=CARTESIAN_POINT('Ctrl Pts',(-1.90335253862834,1.,0.174375518661085));
#27772=CARTESIAN_POINT('Ctrl Pts',(-1.89788101117132,-1.,0.174879405091263));
#27773=CARTESIAN_POINT('Ctrl Pts',(-1.89788101117132,1.,0.174879405091263));
#27774=CARTESIAN_POINT('Ctrl Pts',(-1.892646301985,-1.,0.175274276190844));
#27775=CARTESIAN_POINT('Ctrl Pts',(-1.892646301985,1.,0.175274276190844));
#27776=CARTESIAN_POINT('Ctrl Pts',(-1.88742606273259,-1.,0.175538155840648));
#27777=CARTESIAN_POINT('Ctrl Pts',(-1.88742606273259,1.,0.175538155840648));
#27778=CARTESIAN_POINT('Ctrl Pts',(-1.88188663145367,-1.,0.175644148889698));
#27779=CARTESIAN_POINT('Ctrl Pts',(-1.88188663145367,1.,0.175644148889698));
#27780=CARTESIAN_POINT('Ctrl Pts',(-1.87563767773588,-1.,0.175563480746485));
#27781=CARTESIAN_POINT('Ctrl Pts',(-1.87563767773588,1.,0.175563480746485));
#27782=CARTESIAN_POINT('Ctrl Pts',(-1.86828349694799,-1.,0.175268337590758));
#27783=CARTESIAN_POINT('Ctrl Pts',(-1.86828349694799,1.,0.175268337590758));
#27784=CARTESIAN_POINT('Ctrl Pts',(-1.85948367088837,-1.,0.17473525927603));
#27785=CARTESIAN_POINT('Ctrl Pts',(-1.85948367088837,1.,0.17473525927603));
#27786=CARTESIAN_POINT('Ctrl Pts',(-1.8489811319852,-1.,0.173946627587731));
#27787=CARTESIAN_POINT('Ctrl Pts',(-1.8489811319852,1.,0.173946627587731));
#27788=CARTESIAN_POINT('Ctrl Pts',(-1.83658380527692,-1.,0.1728894428919));
#27789=CARTESIAN_POINT('Ctrl Pts',(-1.83658380527692,1.,0.1728894428919));
#27790=CARTESIAN_POINT('Ctrl Pts',(-1.82215766811545,-1.,0.171554770204119));
#27791=CARTESIAN_POINT('Ctrl Pts',(-1.82215766811545,1.,0.171554770204119));
#27792=CARTESIAN_POINT('Ctrl Pts',(-1.80561530629706,-1.,0.169936923904608));
#27793=CARTESIAN_POINT('Ctrl Pts',(-1.80561530629706,1.,0.169936923904608));
#27794=CARTESIAN_POINT('Ctrl Pts',(-1.7869064998507,-1.,0.168032772805197));
#27795=CARTESIAN_POINT('Ctrl Pts',(-1.7869064998507,1.,0.168032772805197));
#27796=CARTESIAN_POINT('Ctrl Pts',(-1.77018771684844,-1.,0.1662793551464));
#27797=CARTESIAN_POINT('Ctrl Pts',(-1.77018771684844,1.,0.1662793551464));
#27798=CARTESIAN_POINT('Ctrl Pts',(-1.75666056638427,-1.,0.164834765707158));
#27799=CARTESIAN_POINT('Ctrl Pts',(-1.75666056638427,1.,0.164834765707158));
#27800=CARTESIAN_POINT('Ctrl Pts',(-1.7472034950333,-1.,0.163814161002002));
#27801=CARTESIAN_POINT('Ctrl Pts',(-1.7472034950333,1.,0.163814161002002));
#27802=CARTESIAN_POINT('Ctrl Pts',(-1.74236521665491,-1.,0.163289472382896));
#27803=CARTESIAN_POINT('Ctrl Pts',(-1.74236521665491,1.,0.163289472382896));
#27804=CARTESIAN_POINT('',(-2.19890268624765,1.,0.069476445021958));
#27805=CARTESIAN_POINT('Ctrl Pts',(-2.19890268624765,1.,0.069476445021958));
#27806=CARTESIAN_POINT('Ctrl Pts',(-2.19777582085423,1.,0.0701143536325489));
#27807=CARTESIAN_POINT('Ctrl Pts',(-2.19552129484002,1.,0.0713863779526153));
#27808=CARTESIAN_POINT('Ctrl Pts',(-2.19213712013662,1.,0.0732830357306724));
#27809=CARTESIAN_POINT('Ctrl Pts',(-2.1876201139953,1.,0.0757891465836146));
#27810=CARTESIAN_POINT('Ctrl Pts',(-2.18196589448887,1.,0.0788837727685241));
#27811=CARTESIAN_POINT('Ctrl Pts',(-2.176303712113,1.,0.0819402680872764));
#27812=CARTESIAN_POINT('Ctrl Pts',(-2.17063357870952,1.,0.0849584620835371));
#27813=CARTESIAN_POINT('Ctrl Pts',(-2.16495552645014,1.,0.0879381291386921));
#27814=CARTESIAN_POINT('Ctrl Pts',(-2.15926961544516,1.,0.0908789888107264));
#27815=CARTESIAN_POINT('Ctrl Pts',(-2.1535759397817,1.,0.0937807218867642));
#27816=CARTESIAN_POINT('Ctrl Pts',(-2.14787463531795,1.,0.0966429852305457));
#27817=CARTESIAN_POINT('Ctrl Pts',(-2.14216588396025,1.,0.0994654261990914));
#27818=CARTESIAN_POINT('Ctrl Pts',(-2.13644992667165,1.,0.1022477005561));
#27819=CARTESIAN_POINT('Ctrl Pts',(-2.13072704887293,1.,0.104989479152739));
#27820=CARTESIAN_POINT('Ctrl Pts',(-2.12499752307,1.,0.10769043523109));
#27821=CARTESIAN_POINT('Ctrl Pts',(-2.11926155590865,1.,0.110350236135025));
#27822=CARTESIAN_POINT('Ctrl Pts',(-2.11351924490306,1.,0.112968534419737));
#27823=CARTESIAN_POINT('Ctrl Pts',(-2.10777050261309,1.,0.115544957687926));
#27824=CARTESIAN_POINT('Ctrl Pts',(-2.102015121329,1.,0.118079107988355));
#27825=CARTESIAN_POINT('Ctrl Pts',(-2.0962529286773,1.,0.120570567965122));
#27826=CARTESIAN_POINT('Ctrl Pts',(-2.09048392424825,1.,0.123018905621083));
#27827=CARTESIAN_POINT('Ctrl Pts',(-2.08470840653643,1.,0.125423679412061));
#27828=CARTESIAN_POINT('Ctrl Pts',(-2.07892715110987,1.,0.12778444527612));
#27829=CARTESIAN_POINT('Ctrl Pts',(-2.07314114713063,1.,0.130100748328403));
#27830=CARTESIAN_POINT('Ctrl Pts',(-2.06735123910326,1.,0.13237211154771));
#27831=CARTESIAN_POINT('Ctrl Pts',(-2.06155781517842,1.,0.134598026192106));
#27832=CARTESIAN_POINT('Ctrl Pts',(-2.05576044414264,1.,0.136777941218043));
#27833=CARTESIAN_POINT('Ctrl Pts',(-2.04995762001328,1.,0.138911255368966));
#27834=CARTESIAN_POINT('Ctrl Pts',(-2.04414757947916,1.,0.140997332152546));
#27835=CARTESIAN_POINT('Ctrl Pts',(-2.03832911025912,1.,0.143035515058209));
#27836=CARTESIAN_POINT('Ctrl Pts',(-2.03250223739942,1.,0.145025140186057));
#27837=CARTESIAN_POINT('Ctrl Pts',(-2.02666926182017,1.,0.146965557332583));
#27838=CARTESIAN_POINT('Ctrl Pts',(-2.02083464969894,1.,0.148856124775337));
#27839=CARTESIAN_POINT('Ctrl Pts',(-2.01500291940238,1.,0.150696157673078));
#27840=CARTESIAN_POINT('Ctrl Pts',(-2.00917680318424,1.,0.15248488362145));
#27841=CARTESIAN_POINT('Ctrl Pts',(-2.00335565310543,1.,0.154221403049722));
#27842=CARTESIAN_POINT('Ctrl Pts',(-1.99753284771497,1.,0.155904629548783));
#27843=CARTESIAN_POINT('Ctrl Pts',(-1.99169810931908,1.,0.157533331459227));
#27844=CARTESIAN_POINT('Ctrl Pts',(-1.98584238283292,1.,0.159106226437299));
#27845=CARTESIAN_POINT('Ctrl Pts',(-1.97996195437559,1.,0.160622060784611));
#27846=CARTESIAN_POINT('Ctrl Pts',(-1.97406280235188,1.,0.162079693556288));
#27847=CARTESIAN_POINT('Ctrl Pts',(-1.96816512677967,1.,0.163478185457734));
#27848=CARTESIAN_POINT('Ctrl Pts',(-1.96229379940136,1.,0.164816568920269));
#27849=CARTESIAN_POINT('Ctrl Pts',(-1.9564675971873,1.,0.166093592002812));
#27850=CARTESIAN_POINT('Ctrl Pts',(-1.95069027794294,1.,0.167307501784475));
#27851=CARTESIAN_POINT('Ctrl Pts',(-1.94493757756931,1.,0.168455741607556));
#27852=CARTESIAN_POINT('Ctrl Pts',(-1.93915639211581,1.,0.169534904817491));
#27853=CARTESIAN_POINT('Ctrl Pts',(-1.93329183155539,1.,0.170541253116201));
#27854=CARTESIAN_POINT('Ctrl Pts',(-1.92731093582036,1.,0.171471191532988));
#27855=CARTESIAN_POINT('Ctrl Pts',(-1.9212233439798,1.,0.172321621259514));
#27856=CARTESIAN_POINT('Ctrl Pts',(-1.91511429159527,1.,0.173090695383496));
#27857=CARTESIAN_POINT('Ctrl Pts',(-1.90911693975267,1.,0.173776635257817));
#27858=CARTESIAN_POINT('Ctrl Pts',(-1.90335253862834,1.,0.174375518661085));
#27859=CARTESIAN_POINT('Ctrl Pts',(-1.89788101117132,1.,0.174879405091263));
#27860=CARTESIAN_POINT('Ctrl Pts',(-1.892646301985,1.,0.175274276190844));
#27861=CARTESIAN_POINT('Ctrl Pts',(-1.88742606273259,1.,0.175538155840648));
#27862=CARTESIAN_POINT('Ctrl Pts',(-1.88188663145367,1.,0.175644148889698));
#27863=CARTESIAN_POINT('Ctrl Pts',(-1.87563767773588,1.,0.175563480746485));
#27864=CARTESIAN_POINT('Ctrl Pts',(-1.86828349694799,1.,0.175268337590758));
#27865=CARTESIAN_POINT('Ctrl Pts',(-1.85948367088837,1.,0.17473525927603));
#27866=CARTESIAN_POINT('Ctrl Pts',(-1.8489811319852,1.,0.173946627587731));
#27867=CARTESIAN_POINT('Ctrl Pts',(-1.83658380527692,1.,0.1728894428919));
#27868=CARTESIAN_POINT('Ctrl Pts',(-1.82215766811545,1.,0.171554770204119));
#27869=CARTESIAN_POINT('Ctrl Pts',(-1.80561530629706,1.,0.169936923904608));
#27870=CARTESIAN_POINT('Ctrl Pts',(-1.7869064998507,1.,0.168032772805197));
#27871=CARTESIAN_POINT('Ctrl Pts',(-1.77018771684844,1.,0.1662793551464));
#27872=CARTESIAN_POINT('Ctrl Pts',(-1.75666056638427,1.,0.164834765707158));
#27873=CARTESIAN_POINT('Ctrl Pts',(-1.7472034950333,1.,0.163814161002002));
#27874=CARTESIAN_POINT('Ctrl Pts',(-1.74236521665491,1.,0.163289472382896));
#27875=CARTESIAN_POINT('',(-2.19890268624765,0.,0.069476445021958));
#27876=CARTESIAN_POINT('Origin',(-2.19890268624765,0.,-0.0694764450219585));
#27877=CARTESIAN_POINT('',(-2.19890268624765,1.,-0.0694764450219585));
#27878=CARTESIAN_POINT('',(-2.19890268624765,1.,0.069476445021958));
#27879=CARTESIAN_POINT('',(-2.19890268624765,0.,-0.0694764450219585));
#27880=CARTESIAN_POINT('Ctrl Pts',(-1.74236521665491,-1.,-0.163289472382896));
#27881=CARTESIAN_POINT('Ctrl Pts',(-1.74236521665491,1.,-0.163289472382896));
#27882=CARTESIAN_POINT('Ctrl Pts',(-1.74720349503904,-1.,-0.163814161002474));
#27883=CARTESIAN_POINT('Ctrl Pts',(-1.74720349503904,1.,-0.163814161002474));
#27884=CARTESIAN_POINT('Ctrl Pts',(-1.75666056640041,-1.,-0.164834765708484));
#27885=CARTESIAN_POINT('Ctrl Pts',(-1.75666056640041,1.,-0.164834765708484));
#27886=CARTESIAN_POINT('Ctrl Pts',(-1.77018771687692,-1.,-0.166279355148738));
#27887=CARTESIAN_POINT('Ctrl Pts',(-1.77018771687692,1.,-0.166279355148738));
#27888=CARTESIAN_POINT('Ctrl Pts',(-1.78690649988931,-1.,-0.16803277280837));
#27889=CARTESIAN_POINT('Ctrl Pts',(-1.78690649988931,1.,-0.16803277280837));
#27890=CARTESIAN_POINT('Ctrl Pts',(-1.80561530633924,-1.,-0.169936923908078));
#27891=CARTESIAN_POINT('Ctrl Pts',(-1.80561530633924,1.,-0.169936923908078));
#27892=CARTESIAN_POINT('Ctrl Pts',(-1.82215766815414,-1.,-0.171554770207306));
#27893=CARTESIAN_POINT('Ctrl Pts',(-1.82215766815414,1.,-0.171554770207306));
#27894=CARTESIAN_POINT('Ctrl Pts',(-1.83658380530747,-1.,-0.17288944289442));
#27895=CARTESIAN_POINT('Ctrl Pts',(-1.83658380530747,1.,-0.17288944289442));
#27896=CARTESIAN_POINT('Ctrl Pts',(-1.84898113200543,-1.,-0.173946627589401));
#27897=CARTESIAN_POINT('Ctrl Pts',(-1.84898113200543,1.,-0.173946627589401));
#27898=CARTESIAN_POINT('Ctrl Pts',(-1.85948367089838,-1.,-0.174735259276856));
#27899=CARTESIAN_POINT('Ctrl Pts',(-1.85948367089838,1.,-0.174735259276856));
#27900=CARTESIAN_POINT('Ctrl Pts',(-1.86828349694972,-1.,-0.175268337590901));
#27901=CARTESIAN_POINT('Ctrl Pts',(-1.86828349694972,1.,-0.175268337590901));
#27902=CARTESIAN_POINT('Ctrl Pts',(-1.87563767773249,-1.,-0.175563480746205));
#27903=CARTESIAN_POINT('Ctrl Pts',(-1.87563767773249,1.,-0.175563480746205));
#27904=CARTESIAN_POINT('Ctrl Pts',(-1.88188663144846,-1.,-0.175644148889271));
#27905=CARTESIAN_POINT('Ctrl Pts',(-1.88188663144846,1.,-0.175644148889271));
#27906=CARTESIAN_POINT('Ctrl Pts',(-1.88742606272818,-1.,-0.175538155840286));
#27907=CARTESIAN_POINT('Ctrl Pts',(-1.88742606272818,1.,-0.175538155840286));
#27908=CARTESIAN_POINT('Ctrl Pts',(-1.89264630198279,-1.,-0.175274276190664));
#27909=CARTESIAN_POINT('Ctrl Pts',(-1.89264630198279,1.,-0.175274276190664));
#27910=CARTESIAN_POINT('Ctrl Pts',(-1.89788101117148,-1.,-0.174879405091277));
#27911=CARTESIAN_POINT('Ctrl Pts',(-1.89788101117148,1.,-0.174879405091277));
#27912=CARTESIAN_POINT('Ctrl Pts',(-1.90335253863003,-1.,-0.174375518661222));
#27913=CARTESIAN_POINT('Ctrl Pts',(-1.90335253863003,1.,-0.174375518661222));
#27914=CARTESIAN_POINT('Ctrl Pts',(-1.90911693975475,-1.,-0.173776635257984));
#27915=CARTESIAN_POINT('Ctrl Pts',(-1.90911693975475,1.,-0.173776635257984));
#27916=CARTESIAN_POINT('Ctrl Pts',(-1.91511429159681,-1.,-0.173090695383619));
#27917=CARTESIAN_POINT('Ctrl Pts',(-1.91511429159681,1.,-0.173090695383619));
#27918=CARTESIAN_POINT('Ctrl Pts',(-1.92122334398034,-1.,-0.172321621259557));
#27919=CARTESIAN_POINT('Ctrl Pts',(-1.92122334398034,1.,-0.172321621259557));
#27920=CARTESIAN_POINT('Ctrl Pts',(-1.92731093582,-1.,-0.17147119153296));
#27921=CARTESIAN_POINT('Ctrl Pts',(-1.92731093582,1.,-0.17147119153296));
#27922=CARTESIAN_POINT('Ctrl Pts',(-1.93329183155455,-1.,-0.170541253116136));
#27923=CARTESIAN_POINT('Ctrl Pts',(-1.93329183155455,1.,-0.170541253116136));
#27924=CARTESIAN_POINT('Ctrl Pts',(-1.93915639211497,-1.,-0.169534904817425));
#27925=CARTESIAN_POINT('Ctrl Pts',(-1.93915639211497,1.,-0.169534904817425));
#27926=CARTESIAN_POINT('Ctrl Pts',(-1.94493757756879,-1.,-0.168455741607516));
#27927=CARTESIAN_POINT('Ctrl Pts',(-1.94493757756879,1.,-0.168455741607516));
#27928=CARTESIAN_POINT('Ctrl Pts',(-1.95069027794286,-1.,-0.167307501784469));
#27929=CARTESIAN_POINT('Ctrl Pts',(-1.95069027794286,1.,-0.167307501784469));
#27930=CARTESIAN_POINT('Ctrl Pts',(-1.95646759718755,-1.,-0.166093592002833));
#27931=CARTESIAN_POINT('Ctrl Pts',(-1.95646759718755,1.,-0.166093592002833));
#27932=CARTESIAN_POINT('Ctrl Pts',(-1.96229379940174,-1.,-0.1648165689203));
#27933=CARTESIAN_POINT('Ctrl Pts',(-1.96229379940174,1.,-0.1648165689203));
#27934=CARTESIAN_POINT('Ctrl Pts',(-1.96816512678,-1.,-0.16347818545776));
#27935=CARTESIAN_POINT('Ctrl Pts',(-1.96816512678,1.,-0.16347818545776));
#27936=CARTESIAN_POINT('Ctrl Pts',(-1.97406280235204,-1.,-0.162079693556302));
#27937=CARTESIAN_POINT('Ctrl Pts',(-1.97406280235204,1.,-0.162079693556302));
#27938=CARTESIAN_POINT('Ctrl Pts',(-1.97996195437557,-1.,-0.16062206078461));
#27939=CARTESIAN_POINT('Ctrl Pts',(-1.97996195437557,1.,-0.16062206078461));
#27940=CARTESIAN_POINT('Ctrl Pts',(-1.98584238283279,-1.,-0.159106226437289));
#27941=CARTESIAN_POINT('Ctrl Pts',(-1.98584238283279,1.,-0.159106226437289));
#27942=CARTESIAN_POINT('Ctrl Pts',(-1.99169810931893,-1.,-0.157533331459215));
#27943=CARTESIAN_POINT('Ctrl Pts',(-1.99169810931893,1.,-0.157533331459215));
#27944=CARTESIAN_POINT('Ctrl Pts',(-1.99753284771487,-1.,-0.155904629548775));
#27945=CARTESIAN_POINT('Ctrl Pts',(-1.99753284771487,1.,-0.155904629548775));
#27946=CARTESIAN_POINT('Ctrl Pts',(-2.00335565310539,-1.,-0.154221403049719));
#27947=CARTESIAN_POINT('Ctrl Pts',(-2.00335565310539,1.,-0.154221403049719));
#27948=CARTESIAN_POINT('Ctrl Pts',(-2.00917680318426,-1.,-0.152484883621452));
#27949=CARTESIAN_POINT('Ctrl Pts',(-2.00917680318426,1.,-0.152484883621452));
#27950=CARTESIAN_POINT('Ctrl Pts',(-2.01500291940243,-1.,-0.150696157673084));
#27951=CARTESIAN_POINT('Ctrl Pts',(-2.01500291940243,1.,-0.150696157673084));
#27952=CARTESIAN_POINT('Ctrl Pts',(-2.02083464969897,-1.,-0.148856124775343));
#27953=CARTESIAN_POINT('Ctrl Pts',(-2.02083464969897,1.,-0.148856124775343));
#27954=CARTESIAN_POINT('Ctrl Pts',(-2.02666926182017,-1.,-0.146965557332586));
#27955=CARTESIAN_POINT('Ctrl Pts',(-2.02666926182017,1.,-0.146965557332586));
#27956=CARTESIAN_POINT('Ctrl Pts',(-2.03250223739941,-1.,-0.145025140186058));
#27957=CARTESIAN_POINT('Ctrl Pts',(-2.03250223739941,1.,-0.145025140186058));
#27958=CARTESIAN_POINT('Ctrl Pts',(-2.03832911025913,-1.,-0.143035515058208));
#27959=CARTESIAN_POINT('Ctrl Pts',(-2.03832911025913,1.,-0.143035515058208));
#27960=CARTESIAN_POINT('Ctrl Pts',(-2.04414757947919,-1.,-0.140997332152545));
#27961=CARTESIAN_POINT('Ctrl Pts',(-2.04414757947919,1.,-0.140997332152545));
#27962=CARTESIAN_POINT('Ctrl Pts',(-2.04995762001333,-1.,-0.138911255368966));
#27963=CARTESIAN_POINT('Ctrl Pts',(-2.04995762001333,1.,-0.138911255368966));
#27964=CARTESIAN_POINT('Ctrl Pts',(-2.0557604441427,-1.,-0.136777941218044));
#27965=CARTESIAN_POINT('Ctrl Pts',(-2.0557604441427,1.,-0.136777941218044));
#27966=CARTESIAN_POINT('Ctrl Pts',(-2.06155781517844,-1.,-0.134598026192107));
#27967=CARTESIAN_POINT('Ctrl Pts',(-2.06155781517844,1.,-0.134598026192107));
#27968=CARTESIAN_POINT('Ctrl Pts',(-2.06735123910319,-1.,-0.13237211154771));
#27969=CARTESIAN_POINT('Ctrl Pts',(-2.06735123910319,1.,-0.13237211154771));
#27970=CARTESIAN_POINT('Ctrl Pts',(-2.07314114713047,-1.,-0.130100748328401));
#27971=CARTESIAN_POINT('Ctrl Pts',(-2.07314114713047,1.,-0.130100748328401));
#27972=CARTESIAN_POINT('Ctrl Pts',(-2.07892715110967,-1.,-0.127784445276116));
#27973=CARTESIAN_POINT('Ctrl Pts',(-2.07892715110967,1.,-0.127784445276116));
#27974=CARTESIAN_POINT('Ctrl Pts',(-2.08470840653628,-1.,-0.125423679412058));
#27975=CARTESIAN_POINT('Ctrl Pts',(-2.08470840653628,1.,-0.125423679412058));
#27976=CARTESIAN_POINT('Ctrl Pts',(-2.09048392424826,-1.,-0.123018905621083));
#27977=CARTESIAN_POINT('Ctrl Pts',(-2.09048392424826,1.,-0.123018905621083));
#27978=CARTESIAN_POINT('Ctrl Pts',(-2.09625292867756,-1.,-0.120570567965129));
#27979=CARTESIAN_POINT('Ctrl Pts',(-2.09625292867756,1.,-0.120570567965129));
#27980=CARTESIAN_POINT('Ctrl Pts',(-2.10201512132945,-1.,-0.118079107988368));
#27981=CARTESIAN_POINT('Ctrl Pts',(-2.10201512132945,1.,-0.118079107988368));
#27982=CARTESIAN_POINT('Ctrl Pts',(-2.10777050261359,-1.,-0.11554495768794));
#27983=CARTESIAN_POINT('Ctrl Pts',(-2.10777050261359,1.,-0.11554495768794));
#27984=CARTESIAN_POINT('Ctrl Pts',(-2.11351924490335,-1.,-0.112968534419746));
#27985=CARTESIAN_POINT('Ctrl Pts',(-2.11351924490335,1.,-0.112968534419746));
#27986=CARTESIAN_POINT('Ctrl Pts',(-2.11926155590849,-1.,-0.11035023613502));
#27987=CARTESIAN_POINT('Ctrl Pts',(-2.11926155590849,1.,-0.11035023613502));
#27988=CARTESIAN_POINT('Ctrl Pts',(-2.12499752306927,-1.,-0.107690435231068));
#27989=CARTESIAN_POINT('Ctrl Pts',(-2.12499752306927,1.,-0.107690435231068));
#27990=CARTESIAN_POINT('Ctrl Pts',(-2.1307270488718,-1.,-0.104989479152703));
#27991=CARTESIAN_POINT('Ctrl Pts',(-2.1307270488718,1.,-0.104989479152703));
#27992=CARTESIAN_POINT('Ctrl Pts',(-2.13644992667052,-1.,-0.102247700556064));
#27993=CARTESIAN_POINT('Ctrl Pts',(-2.13644992667052,1.,-0.102247700556064));
#27994=CARTESIAN_POINT('Ctrl Pts',(-2.14216588395974,-1.,-0.0994654261990744));
#27995=CARTESIAN_POINT('Ctrl Pts',(-2.14216588395974,1.,-0.0994654261990744));
#27996=CARTESIAN_POINT('Ctrl Pts',(-2.14787463531864,-1.,-0.096642985230569));
#27997=CARTESIAN_POINT('Ctrl Pts',(-2.14787463531864,1.,-0.096642985230569));
#27998=CARTESIAN_POINT('Ctrl Pts',(-2.15357593978377,-1.,-0.0937807218868346));
#27999=CARTESIAN_POINT('Ctrl Pts',(-2.15357593978377,1.,-0.0937807218868346));
#28000=CARTESIAN_POINT('Ctrl Pts',(-2.15926961544808,-1.,-0.0908789888108267));
#28001=CARTESIAN_POINT('Ctrl Pts',(-2.15926961544808,1.,-0.0908789888108267));
#28002=CARTESIAN_POINT('Ctrl Pts',(-2.16495552645275,-1.,-0.0879381291387824));
#28003=CARTESIAN_POINT('Ctrl Pts',(-2.16495552645275,1.,-0.0879381291387824));
#28004=CARTESIAN_POINT('Ctrl Pts',(-2.17063357871031,-1.,-0.0849584620835644));
#28005=CARTESIAN_POINT('Ctrl Pts',(-2.17063357871031,1.,-0.0849584620835644));
#28006=CARTESIAN_POINT('Ctrl Pts',(-2.1763037121106,-1.,-0.0819402680871941));
#28007=CARTESIAN_POINT('Ctrl Pts',(-2.1763037121106,1.,-0.0819402680871941));
#28008=CARTESIAN_POINT('Ctrl Pts',(-2.18196589448304,-1.,-0.0788837727683229));
#28009=CARTESIAN_POINT('Ctrl Pts',(-2.18196589448304,1.,-0.0788837727683229));
#28010=CARTESIAN_POINT('Ctrl Pts',(-2.1876201139874,-1.,-0.0757891465833413));
#28011=CARTESIAN_POINT('Ctrl Pts',(-2.1876201139874,1.,-0.0757891465833413));
#28012=CARTESIAN_POINT('Ctrl Pts',(-2.19213712012956,-1.,-0.0732830357304277));
#28013=CARTESIAN_POINT('Ctrl Pts',(-2.19213712012956,1.,-0.0732830357304277));
#28014=CARTESIAN_POINT('Ctrl Pts',(-2.19552129483562,-1.,-0.0713863779524629));
#28015=CARTESIAN_POINT('Ctrl Pts',(-2.19552129483562,1.,-0.0713863779524629));
#28016=CARTESIAN_POINT('Ctrl Pts',(-2.19777582085261,-1.,-0.0701143536324927));
#28017=CARTESIAN_POINT('Ctrl Pts',(-2.19777582085261,1.,-0.0701143536324927));
#28018=CARTESIAN_POINT('Ctrl Pts',(-2.19890268624765,-1.,-0.0694764450219585));
#28019=CARTESIAN_POINT('Ctrl Pts',(-2.19890268624765,1.,-0.0694764450219585));
#28020=CARTESIAN_POINT('',(-1.74236521665491,1.,-0.163289472382896));
#28021=CARTESIAN_POINT('Ctrl Pts',(-1.74236521665491,1.,-0.163289472382896));
#28022=CARTESIAN_POINT('Ctrl Pts',(-1.74720349503904,1.,-0.163814161002474));
#28023=CARTESIAN_POINT('Ctrl Pts',(-1.75666056640041,1.,-0.164834765708484));
#28024=CARTESIAN_POINT('Ctrl Pts',(-1.77018771687692,1.,-0.166279355148738));
#28025=CARTESIAN_POINT('Ctrl Pts',(-1.78690649988931,1.,-0.16803277280837));
#28026=CARTESIAN_POINT('Ctrl Pts',(-1.80561530633924,1.,-0.169936923908078));
#28027=CARTESIAN_POINT('Ctrl Pts',(-1.82215766815414,1.,-0.171554770207306));
#28028=CARTESIAN_POINT('Ctrl Pts',(-1.83658380530747,1.,-0.17288944289442));
#28029=CARTESIAN_POINT('Ctrl Pts',(-1.84898113200543,1.,-0.173946627589401));
#28030=CARTESIAN_POINT('Ctrl Pts',(-1.85948367089838,1.,-0.174735259276856));
#28031=CARTESIAN_POINT('Ctrl Pts',(-1.86828349694972,1.,-0.175268337590901));
#28032=CARTESIAN_POINT('Ctrl Pts',(-1.87563767773249,1.,-0.175563480746205));
#28033=CARTESIAN_POINT('Ctrl Pts',(-1.88188663144846,1.,-0.175644148889271));
#28034=CARTESIAN_POINT('Ctrl Pts',(-1.88742606272818,1.,-0.175538155840286));
#28035=CARTESIAN_POINT('Ctrl Pts',(-1.89264630198279,1.,-0.175274276190664));
#28036=CARTESIAN_POINT('Ctrl Pts',(-1.89788101117148,1.,-0.174879405091277));
#28037=CARTESIAN_POINT('Ctrl Pts',(-1.90335253863003,1.,-0.174375518661222));
#28038=CARTESIAN_POINT('Ctrl Pts',(-1.90911693975475,1.,-0.173776635257984));
#28039=CARTESIAN_POINT('Ctrl Pts',(-1.91511429159681,1.,-0.173090695383619));
#28040=CARTESIAN_POINT('Ctrl Pts',(-1.92122334398034,1.,-0.172321621259557));
#28041=CARTESIAN_POINT('Ctrl Pts',(-1.92731093582,1.,-0.17147119153296));
#28042=CARTESIAN_POINT('Ctrl Pts',(-1.93329183155455,1.,-0.170541253116136));
#28043=CARTESIAN_POINT('Ctrl Pts',(-1.93915639211497,1.,-0.169534904817425));
#28044=CARTESIAN_POINT('Ctrl Pts',(-1.94493757756879,1.,-0.168455741607516));
#28045=CARTESIAN_POINT('Ctrl Pts',(-1.95069027794286,1.,-0.167307501784469));
#28046=CARTESIAN_POINT('Ctrl Pts',(-1.95646759718755,1.,-0.166093592002833));
#28047=CARTESIAN_POINT('Ctrl Pts',(-1.96229379940174,1.,-0.1648165689203));
#28048=CARTESIAN_POINT('Ctrl Pts',(-1.96816512678,1.,-0.16347818545776));
#28049=CARTESIAN_POINT('Ctrl Pts',(-1.97406280235204,1.,-0.162079693556302));
#28050=CARTESIAN_POINT('Ctrl Pts',(-1.97996195437557,1.,-0.16062206078461));
#28051=CARTESIAN_POINT('Ctrl Pts',(-1.98584238283279,1.,-0.159106226437289));
#28052=CARTESIAN_POINT('Ctrl Pts',(-1.99169810931893,1.,-0.157533331459215));
#28053=CARTESIAN_POINT('Ctrl Pts',(-1.99753284771487,1.,-0.155904629548775));
#28054=CARTESIAN_POINT('Ctrl Pts',(-2.00335565310539,1.,-0.154221403049719));
#28055=CARTESIAN_POINT('Ctrl Pts',(-2.00917680318426,1.,-0.152484883621452));
#28056=CARTESIAN_POINT('Ctrl Pts',(-2.01500291940243,1.,-0.150696157673084));
#28057=CARTESIAN_POINT('Ctrl Pts',(-2.02083464969897,1.,-0.148856124775343));
#28058=CARTESIAN_POINT('Ctrl Pts',(-2.02666926182017,1.,-0.146965557332586));
#28059=CARTESIAN_POINT('Ctrl Pts',(-2.03250223739941,1.,-0.145025140186058));
#28060=CARTESIAN_POINT('Ctrl Pts',(-2.03832911025913,1.,-0.143035515058208));
#28061=CARTESIAN_POINT('Ctrl Pts',(-2.04414757947919,1.,-0.140997332152545));
#28062=CARTESIAN_POINT('Ctrl Pts',(-2.04995762001333,1.,-0.138911255368966));
#28063=CARTESIAN_POINT('Ctrl Pts',(-2.0557604441427,1.,-0.136777941218044));
#28064=CARTESIAN_POINT('Ctrl Pts',(-2.06155781517844,1.,-0.134598026192107));
#28065=CARTESIAN_POINT('Ctrl Pts',(-2.06735123910319,1.,-0.13237211154771));
#28066=CARTESIAN_POINT('Ctrl Pts',(-2.07314114713047,1.,-0.130100748328401));
#28067=CARTESIAN_POINT('Ctrl Pts',(-2.07892715110967,1.,-0.127784445276116));
#28068=CARTESIAN_POINT('Ctrl Pts',(-2.08470840653628,1.,-0.125423679412058));
#28069=CARTESIAN_POINT('Ctrl Pts',(-2.09048392424826,1.,-0.123018905621083));
#28070=CARTESIAN_POINT('Ctrl Pts',(-2.09625292867756,1.,-0.120570567965129));
#28071=CARTESIAN_POINT('Ctrl Pts',(-2.10201512132945,1.,-0.118079107988368));
#28072=CARTESIAN_POINT('Ctrl Pts',(-2.10777050261359,1.,-0.11554495768794));
#28073=CARTESIAN_POINT('Ctrl Pts',(-2.11351924490335,1.,-0.112968534419746));
#28074=CARTESIAN_POINT('Ctrl Pts',(-2.11926155590849,1.,-0.11035023613502));
#28075=CARTESIAN_POINT('Ctrl Pts',(-2.12499752306927,1.,-0.107690435231068));
#28076=CARTESIAN_POINT('Ctrl Pts',(-2.1307270488718,1.,-0.104989479152703));
#28077=CARTESIAN_POINT('Ctrl Pts',(-2.13644992667052,1.,-0.102247700556064));
#28078=CARTESIAN_POINT('Ctrl Pts',(-2.14216588395974,1.,-0.0994654261990744));
#28079=CARTESIAN_POINT('Ctrl Pts',(-2.14787463531864,1.,-0.096642985230569));
#28080=CARTESIAN_POINT('Ctrl Pts',(-2.15357593978377,1.,-0.0937807218868346));
#28081=CARTESIAN_POINT('Ctrl Pts',(-2.15926961544808,1.,-0.0908789888108267));
#28082=CARTESIAN_POINT('Ctrl Pts',(-2.16495552645275,1.,-0.0879381291387824));
#28083=CARTESIAN_POINT('Ctrl Pts',(-2.17063357871031,1.,-0.0849584620835644));
#28084=CARTESIAN_POINT('Ctrl Pts',(-2.1763037121106,1.,-0.0819402680871941));
#28085=CARTESIAN_POINT('Ctrl Pts',(-2.18196589448304,1.,-0.0788837727683229));
#28086=CARTESIAN_POINT('Ctrl Pts',(-2.1876201139874,1.,-0.0757891465833413));
#28087=CARTESIAN_POINT('Ctrl Pts',(-2.19213712012956,1.,-0.0732830357304277));
#28088=CARTESIAN_POINT('Ctrl Pts',(-2.19552129483562,1.,-0.0713863779524629));
#28089=CARTESIAN_POINT('Ctrl Pts',(-2.19777582085261,1.,-0.0701143536324927));
#28090=CARTESIAN_POINT('Ctrl Pts',(-2.19890268624765,1.,-0.0694764450219585));
#28091=CARTESIAN_POINT('',(-1.74236521665491,0.,-0.163289472382896));
#28092=CARTESIAN_POINT('Origin',(0.,0.,0.));
#28093=CARTESIAN_POINT('',(-1.7075470150345,1.,-0.383122945602004));
#28094=CARTESIAN_POINT('Origin',(0.,1.,0.));
#28095=CARTESIAN_POINT('',(-1.7075470150345,0.,-0.383122945602004));
#28096=CARTESIAN_POINT('Ctrl Pts',(-2.11275013067528,-1.,-0.61342227326009));
#28097=CARTESIAN_POINT('Ctrl Pts',(-2.11275013067528,1.,-0.61342227326009));
#28098=CARTESIAN_POINT('Ctrl Pts',(-2.11187554260142,-1.,-0.61246736556225));
#28099=CARTESIAN_POINT('Ctrl Pts',(-2.11187554260142,1.,-0.61246736556225));
#28100=CARTESIAN_POINT('Ctrl Pts',(-2.11012443807661,-1.,-0.610560911691113));
#28101=CARTESIAN_POINT('Ctrl Pts',(-2.11012443807661,1.,-0.610560911691113));
#28102=CARTESIAN_POINT('Ctrl Pts',(-2.10749199615859,-1.,-0.607711315456826));
#28103=CARTESIAN_POINT('Ctrl Pts',(-2.10749199615859,1.,-0.607711315456826));
#28104=CARTESIAN_POINT('Ctrl Pts',(-2.10397049887709,-1.,-0.603932030738212));
#28105=CARTESIAN_POINT('Ctrl Pts',(-2.10397049887709,1.,-0.603932030738212));
#28106=CARTESIAN_POINT('Ctrl Pts',(-2.09954930865331,-1.,-0.599241616422144));
#28107=CARTESIAN_POINT('Ctrl Pts',(-2.09954930865331,1.,-0.599241616422144));
#28108=CARTESIAN_POINT('Ctrl Pts',(-2.09510876220501,-1.,-0.594585006052823));
#28109=CARTESIAN_POINT('Ctrl Pts',(-2.09510876220501,1.,-0.594585006052823));
#28110=CARTESIAN_POINT('Ctrl Pts',(-2.09064881812053,-1.,-0.589962365403189));
#28111=CARTESIAN_POINT('Ctrl Pts',(-2.09064881812053,1.,-0.589962365403189));
#28112=CARTESIAN_POINT('Ctrl Pts',(-2.086169437277,-1.,-0.585373918990895));
#28113=CARTESIAN_POINT('Ctrl Pts',(-2.086169437277,1.,-0.585373918990895));
#28114=CARTESIAN_POINT('Ctrl Pts',(-2.08167059018138,-1.,-0.580819952107257));
#28115=CARTESIAN_POINT('Ctrl Pts',(-2.08167059018138,1.,-0.580819952107257));
#28116=CARTESIAN_POINT('Ctrl Pts',(-2.07715226767361,-1.,-0.576300797416274));
#28117=CARTESIAN_POINT('Ctrl Pts',(-2.07715226767361,1.,-0.576300797416274));
#28118=CARTESIAN_POINT('Ctrl Pts',(-2.07261449292757,-1.,-0.571816823242411));
#28119=CARTESIAN_POINT('Ctrl Pts',(-2.07261449292757,1.,-0.571816823242411));
#28120=CARTESIAN_POINT('Ctrl Pts',(-2.06805732997383,-1.,-0.567368421181229));
#28121=CARTESIAN_POINT('Ctrl Pts',(-2.06805732997383,1.,-0.567368421181229));
#28122=CARTESIAN_POINT('Ctrl Pts',(-2.06348090160697,-1.,-0.562955993082574));
#28123=CARTESIAN_POINT('Ctrl Pts',(-2.06348090160697,1.,-0.562955993082574));
#28124=CARTESIAN_POINT('Ctrl Pts',(-2.05888537756571,-1.,-0.558579940185467));
#28125=CARTESIAN_POINT('Ctrl Pts',(-2.05888537756571,1.,-0.558579940185467));
#28126=CARTESIAN_POINT('Ctrl Pts',(-2.05427091604482,-1.,-0.554240657464109));
#28127=CARTESIAN_POINT('Ctrl Pts',(-2.05427091604482,1.,-0.554240657464109));
#28128=CARTESIAN_POINT('Ctrl Pts',(-2.04963761077974,-1.,-0.549938525150342));
#28129=CARTESIAN_POINT('Ctrl Pts',(-2.04963761077974,1.,-0.549938525150342));
#28130=CARTESIAN_POINT('Ctrl Pts',(-2.0449854471456,-1.,-0.545673903817348));
#28131=CARTESIAN_POINT('Ctrl Pts',(-2.0449854471456,1.,-0.545673903817348));
#28132=CARTESIAN_POINT('Ctrl Pts',(-2.0403142269048,-1.,-0.54144712061552));
#28133=CARTESIAN_POINT('Ctrl Pts',(-2.0403142269048,1.,-0.54144712061552));
#28134=CARTESIAN_POINT('Ctrl Pts',(-2.03562362953993,-1.,-0.537258489833134));
#28135=CARTESIAN_POINT('Ctrl Pts',(-2.03562362953993,1.,-0.537258489833134));
#28136=CARTESIAN_POINT('Ctrl Pts',(-2.03091336214401,-1.,-0.533108355132905));
#28137=CARTESIAN_POINT('Ctrl Pts',(-2.03091336214401,1.,-0.533108355132905));
#28138=CARTESIAN_POINT('Ctrl Pts',(-2.02618329083289,-1.,-0.52899712724191));
#28139=CARTESIAN_POINT('Ctrl Pts',(-2.02618329083289,1.,-0.52899712724191));
#28140=CARTESIAN_POINT('Ctrl Pts',(-2.02143356304712,-1.,-0.524925318333518));
#28141=CARTESIAN_POINT('Ctrl Pts',(-2.02143356304712,1.,-0.524925318333518));
#28142=CARTESIAN_POINT('Ctrl Pts',(-2.01666477917305,-1.,-0.520893590399428));
#28143=CARTESIAN_POINT('Ctrl Pts',(-2.01666477917305,1.,-0.520893590399428));
#28144=CARTESIAN_POINT('Ctrl Pts',(-2.01187773939257,-1.,-0.516902681728733));
#28145=CARTESIAN_POINT('Ctrl Pts',(-2.01187773939257,1.,-0.516902681728733));
#28146=CARTESIAN_POINT('Ctrl Pts',(-2.00707309946955,-1.,-0.512953306961813));
#28147=CARTESIAN_POINT('Ctrl Pts',(-2.00707309946955,1.,-0.512953306961813));
#28148=CARTESIAN_POINT('Ctrl Pts',(-2.00225107134733,-1.,-0.509046069886152));
#28149=CARTESIAN_POINT('Ctrl Pts',(-2.00225107134733,1.,-0.509046069886152));
#28150=CARTESIAN_POINT('Ctrl Pts',(-1.99741107463567,-1.,-0.505181361323011));
#28151=CARTESIAN_POINT('Ctrl Pts',(-1.99741107463567,1.,-0.505181361323011));
#28152=CARTESIAN_POINT('Ctrl Pts',(-1.9925514912615,-1.,-0.501359287727129));
#28153=CARTESIAN_POINT('Ctrl Pts',(-1.9925514912615,1.,-0.501359287727129));
#28154=CARTESIAN_POINT('Ctrl Pts',(-1.98767044752929,-1.,-0.497579909545564));
#28155=CARTESIAN_POINT('Ctrl Pts',(-1.98767044752929,1.,-0.497579909545564));
#28156=CARTESIAN_POINT('Ctrl Pts',(-1.9827665876182,-1.,-0.493843476541492));
#28157=CARTESIAN_POINT('Ctrl Pts',(-1.9827665876182,1.,-0.493843476541492));
#28158=CARTESIAN_POINT('Ctrl Pts',(-1.97783973019229,-1.,-0.490150627860955));
#28159=CARTESIAN_POINT('Ctrl Pts',(-1.97783973019229,1.,-0.490150627860955));
#28160=CARTESIAN_POINT('Ctrl Pts',(-1.97289186263272,-1.,-0.486502692907661));
#28161=CARTESIAN_POINT('Ctrl Pts',(-1.97289186263272,1.,-0.486502692907661));
#28162=CARTESIAN_POINT('Ctrl Pts',(-1.96792703422358,-1.,-0.482901662120686));
#28163=CARTESIAN_POINT('Ctrl Pts',(-1.96792703422358,1.,-0.482901662120686));
#28164=CARTESIAN_POINT('Ctrl Pts',(-1.96294933055938,-1.,-0.479349583074846));
#28165=CARTESIAN_POINT('Ctrl Pts',(-1.96294933055938,1.,-0.479349583074846));
#28166=CARTESIAN_POINT('Ctrl Pts',(-1.95796111148175,-1.,-0.475848034683171));
#28167=CARTESIAN_POINT('Ctrl Pts',(-1.95796111148175,1.,-0.475848034683171));
#28168=CARTESIAN_POINT('Ctrl Pts',(-1.95296148278136,-1.,-0.472397672264079));
#28169=CARTESIAN_POINT('Ctrl Pts',(-1.95296148278136,1.,-0.472397672264079));
#28170=CARTESIAN_POINT('Ctrl Pts',(-1.94794381136524,-1.,-0.468997482913158));
#28171=CARTESIAN_POINT('Ctrl Pts',(-1.94794381136524,1.,-0.468997482913158));
#28172=CARTESIAN_POINT('Ctrl Pts',(-1.94289794196205,-1.,-0.465645462026064));
#28173=CARTESIAN_POINT('Ctrl Pts',(-1.94289794196205,1.,-0.465645462026064));
#28174=CARTESIAN_POINT('Ctrl Pts',(-1.93781486640834,-1.,-0.462340031009087));
#28175=CARTESIAN_POINT('Ctrl Pts',(-1.93781486640834,1.,-0.462340031009087));
#28176=CARTESIAN_POINT('Ctrl Pts',(-1.93269066517936,-1.,-0.459081234547931));
#28177=CARTESIAN_POINT('Ctrl Pts',(-1.93269066517936,1.,-0.459081234547931));
#28178=CARTESIAN_POINT('Ctrl Pts',(-1.92753067150461,-1.,-0.455872005174335));
#28179=CARTESIAN_POINT('Ctrl Pts',(-1.92753067150461,1.,-0.455872005174335));
#28180=CARTESIAN_POINT('Ctrl Pts',(-1.9223538064847,-1.,-0.452719478359356));
#28181=CARTESIAN_POINT('Ctrl Pts',(-1.9223538064847,1.,-0.452719478359356));
#28182=CARTESIAN_POINT('Ctrl Pts',(-1.91718342555717,-1.,-0.449632260106572));
#28183=CARTESIAN_POINT('Ctrl Pts',(-1.91718342555717,1.,-0.449632260106572));
#28184=CARTESIAN_POINT('Ctrl Pts',(-1.91203699981095,-1.,-0.446617343485651));
#28185=CARTESIAN_POINT('Ctrl Pts',(-1.91203699981095,1.,-0.446617343485651));
#28186=CARTESIAN_POINT('Ctrl Pts',(-1.90691756144906,-1.,-0.44367755684917));
#28187=CARTESIAN_POINT('Ctrl Pts',(-1.90691756144906,1.,-0.44367755684917));
#28188=CARTESIAN_POINT('Ctrl Pts',(-1.90180124389137,-1.,-0.44080783370416));
#28189=CARTESIAN_POINT('Ctrl Pts',(-1.90180124389137,1.,-0.44080783370416));
#28190=CARTESIAN_POINT('Ctrl Pts',(-1.89663648956549,-1.,-0.437995003948443));
#28191=CARTESIAN_POINT('Ctrl Pts',(-1.89663648956549,1.,-0.437995003948443));
#28192=CARTESIAN_POINT('Ctrl Pts',(-1.89136993975585,-1.,-0.43522566096358));
#28193=CARTESIAN_POINT('Ctrl Pts',(-1.89136993975585,1.,-0.43522566096358));
#28194=CARTESIAN_POINT('Ctrl Pts',(-1.88596913666828,-1.,-0.432493038548833));
#28195=CARTESIAN_POINT('Ctrl Pts',(-1.88596913666828,1.,-0.432493038548833));
#28196=CARTESIAN_POINT('Ctrl Pts',(-1.88044229001778,-1.,-0.429803062482217));
#28197=CARTESIAN_POINT('Ctrl Pts',(-1.88044229001778,1.,-0.429803062482217));
#28198=CARTESIAN_POINT('Ctrl Pts',(-1.87486989291333,-1.,-0.427183828518743));
#28199=CARTESIAN_POINT('Ctrl Pts',(-1.87486989291333,1.,-0.427183828518743));
#28200=CARTESIAN_POINT('Ctrl Pts',(-1.8693780394412,-1.,-0.424678177290876));
#28201=CARTESIAN_POINT('Ctrl Pts',(-1.8693780394412,1.,-0.424678177290876));
#28202=CARTESIAN_POINT('Ctrl Pts',(-1.86408083333863,-1.,-0.422327307417884));
#28203=CARTESIAN_POINT('Ctrl Pts',(-1.86408083333863,1.,-0.422327307417884));
#28204=CARTESIAN_POINT('Ctrl Pts',(-1.8590328109667,-1.,-0.420157287975583));
#28205=CARTESIAN_POINT('Ctrl Pts',(-1.8590328109667,1.,-0.420157287975583));
#28206=CARTESIAN_POINT('Ctrl Pts',(-1.8541763285645,-1.,-0.418164129144045));
#28207=CARTESIAN_POINT('Ctrl Pts',(-1.8541763285645,1.,-0.418164129144045));
#28208=CARTESIAN_POINT('Ctrl Pts',(-1.84929312930314,-1.,-0.416300022039885));
#28209=CARTESIAN_POINT('Ctrl Pts',(-1.84929312930314,1.,-0.416300022039885));
#28210=CARTESIAN_POINT('Ctrl Pts',(-1.84405757074218,-1.,-0.414487438255542));
#28211=CARTESIAN_POINT('Ctrl Pts',(-1.84405757074218,1.,-0.414487438255542));
#28212=CARTESIAN_POINT('Ctrl Pts',(-1.8380895347617,-1.,-0.412633125322945));
#28213=CARTESIAN_POINT('Ctrl Pts',(-1.8380895347617,1.,-0.412633125322945));
#28214=CARTESIAN_POINT('Ctrl Pts',(-1.83100408895047,-1.,-0.410641256301276));
#28215=CARTESIAN_POINT('Ctrl Pts',(-1.83100408895047,1.,-0.410641256301276));
#28216=CARTESIAN_POINT('Ctrl Pts',(-1.82247022677562,-1.,-0.408428948106227));
#28217=CARTESIAN_POINT('Ctrl Pts',(-1.82247022677562,1.,-0.408428948106227));
#28218=CARTESIAN_POINT('Ctrl Pts',(-1.81223801812013,-1.,-0.405933518407175));
#28219=CARTESIAN_POINT('Ctrl Pts',(-1.81223801812013,1.,-0.405933518407175));
#28220=CARTESIAN_POINT('Ctrl Pts',(-1.80012077173238,-1.,-0.403107976163396));
#28221=CARTESIAN_POINT('Ctrl Pts',(-1.80012077173238,1.,-0.403107976163396));
#28222=CARTESIAN_POINT('Ctrl Pts',(-1.78598826343754,-1.,-0.399919403774155));
#28223=CARTESIAN_POINT('Ctrl Pts',(-1.78598826343754,1.,-0.399919403774155));
#28224=CARTESIAN_POINT('Ctrl Pts',(-1.76975560043442,-1.,-0.396346196110688));
#28225=CARTESIAN_POINT('Ctrl Pts',(-1.76975560043442,1.,-0.396346196110688));
#28226=CARTESIAN_POINT('Ctrl Pts',(-1.75137405310193,-1.,-0.392375812285395));
#28227=CARTESIAN_POINT('Ctrl Pts',(-1.75137405310193,1.,-0.392375812285395));
#28228=CARTESIAN_POINT('Ctrl Pts',(-1.73493170972829,-1.,-0.388877023502615));
#28229=CARTESIAN_POINT('Ctrl Pts',(-1.73493170972829,1.,-0.388877023502615));
#28230=CARTESIAN_POINT('Ctrl Pts',(-1.72162022244582,-1.,-0.386070790323281));
#28231=CARTESIAN_POINT('Ctrl Pts',(-1.72162022244582,1.,-0.386070790323281));
#28232=CARTESIAN_POINT('Ctrl Pts',(-1.71231062891398,-1.,-0.384119047314215));
#28233=CARTESIAN_POINT('Ctrl Pts',(-1.71231062891398,1.,-0.384119047314215));
#28234=CARTESIAN_POINT('Ctrl Pts',(-1.7075470150345,-1.,-0.383122945602004));
#28235=CARTESIAN_POINT('Ctrl Pts',(-1.7075470150345,1.,-0.383122945602004));
#28236=CARTESIAN_POINT('',(-2.11275013067528,1.,-0.61342227326009));
#28237=CARTESIAN_POINT('Ctrl Pts',(-2.11275013067528,1.,-0.61342227326009));
#28238=CARTESIAN_POINT('Ctrl Pts',(-2.11187554260142,1.,-0.61246736556225));
#28239=CARTESIAN_POINT('Ctrl Pts',(-2.11012443807661,1.,-0.610560911691113));
#28240=CARTESIAN_POINT('Ctrl Pts',(-2.10749199615859,1.,-0.607711315456826));
#28241=CARTESIAN_POINT('Ctrl Pts',(-2.10397049887709,1.,-0.603932030738212));
#28242=CARTESIAN_POINT('Ctrl Pts',(-2.09954930865331,1.,-0.599241616422144));
#28243=CARTESIAN_POINT('Ctrl Pts',(-2.09510876220501,1.,-0.594585006052823));
#28244=CARTESIAN_POINT('Ctrl Pts',(-2.09064881812053,1.,-0.589962365403189));
#28245=CARTESIAN_POINT('Ctrl Pts',(-2.086169437277,1.,-0.585373918990895));
#28246=CARTESIAN_POINT('Ctrl Pts',(-2.08167059018138,1.,-0.580819952107257));
#28247=CARTESIAN_POINT('Ctrl Pts',(-2.07715226767361,1.,-0.576300797416274));
#28248=CARTESIAN_POINT('Ctrl Pts',(-2.07261449292757,1.,-0.571816823242411));
#28249=CARTESIAN_POINT('Ctrl Pts',(-2.06805732997383,1.,-0.567368421181229));
#28250=CARTESIAN_POINT('Ctrl Pts',(-2.06348090160697,1.,-0.562955993082574));
#28251=CARTESIAN_POINT('Ctrl Pts',(-2.05888537756571,1.,-0.558579940185467));
#28252=CARTESIAN_POINT('Ctrl Pts',(-2.05427091604482,1.,-0.554240657464109));
#28253=CARTESIAN_POINT('Ctrl Pts',(-2.04963761077974,1.,-0.549938525150342));
#28254=CARTESIAN_POINT('Ctrl Pts',(-2.0449854471456,1.,-0.545673903817348));
#28255=CARTESIAN_POINT('Ctrl Pts',(-2.0403142269048,1.,-0.54144712061552));
#28256=CARTESIAN_POINT('Ctrl Pts',(-2.03562362953993,1.,-0.537258489833134));
#28257=CARTESIAN_POINT('Ctrl Pts',(-2.03091336214401,1.,-0.533108355132905));
#28258=CARTESIAN_POINT('Ctrl Pts',(-2.02618329083289,1.,-0.52899712724191));
#28259=CARTESIAN_POINT('Ctrl Pts',(-2.02143356304712,1.,-0.524925318333518));
#28260=CARTESIAN_POINT('Ctrl Pts',(-2.01666477917305,1.,-0.520893590399428));
#28261=CARTESIAN_POINT('Ctrl Pts',(-2.01187773939257,1.,-0.516902681728733));
#28262=CARTESIAN_POINT('Ctrl Pts',(-2.00707309946955,1.,-0.512953306961813));
#28263=CARTESIAN_POINT('Ctrl Pts',(-2.00225107134733,1.,-0.509046069886152));
#28264=CARTESIAN_POINT('Ctrl Pts',(-1.99741107463567,1.,-0.505181361323011));
#28265=CARTESIAN_POINT('Ctrl Pts',(-1.9925514912615,1.,-0.501359287727129));
#28266=CARTESIAN_POINT('Ctrl Pts',(-1.98767044752929,1.,-0.497579909545564));
#28267=CARTESIAN_POINT('Ctrl Pts',(-1.9827665876182,1.,-0.493843476541492));
#28268=CARTESIAN_POINT('Ctrl Pts',(-1.97783973019229,1.,-0.490150627860955));
#28269=CARTESIAN_POINT('Ctrl Pts',(-1.97289186263272,1.,-0.486502692907661));
#28270=CARTESIAN_POINT('Ctrl Pts',(-1.96792703422358,1.,-0.482901662120686));
#28271=CARTESIAN_POINT('Ctrl Pts',(-1.96294933055938,1.,-0.479349583074846));
#28272=CARTESIAN_POINT('Ctrl Pts',(-1.95796111148175,1.,-0.475848034683171));
#28273=CARTESIAN_POINT('Ctrl Pts',(-1.95296148278136,1.,-0.472397672264079));
#28274=CARTESIAN_POINT('Ctrl Pts',(-1.94794381136524,1.,-0.468997482913158));
#28275=CARTESIAN_POINT('Ctrl Pts',(-1.94289794196205,1.,-0.465645462026064));
#28276=CARTESIAN_POINT('Ctrl Pts',(-1.93781486640834,1.,-0.462340031009087));
#28277=CARTESIAN_POINT('Ctrl Pts',(-1.93269066517936,1.,-0.459081234547931));
#28278=CARTESIAN_POINT('Ctrl Pts',(-1.92753067150461,1.,-0.455872005174335));
#28279=CARTESIAN_POINT('Ctrl Pts',(-1.9223538064847,1.,-0.452719478359356));
#28280=CARTESIAN_POINT('Ctrl Pts',(-1.91718342555717,1.,-0.449632260106572));
#28281=CARTESIAN_POINT('Ctrl Pts',(-1.91203699981095,1.,-0.446617343485651));
#28282=CARTESIAN_POINT('Ctrl Pts',(-1.90691756144906,1.,-0.44367755684917));
#28283=CARTESIAN_POINT('Ctrl Pts',(-1.90180124389137,1.,-0.44080783370416));
#28284=CARTESIAN_POINT('Ctrl Pts',(-1.89663648956549,1.,-0.437995003948443));
#28285=CARTESIAN_POINT('Ctrl Pts',(-1.89136993975585,1.,-0.43522566096358));
#28286=CARTESIAN_POINT('Ctrl Pts',(-1.88596913666828,1.,-0.432493038548833));
#28287=CARTESIAN_POINT('Ctrl Pts',(-1.88044229001778,1.,-0.429803062482217));
#28288=CARTESIAN_POINT('Ctrl Pts',(-1.87486989291333,1.,-0.427183828518743));
#28289=CARTESIAN_POINT('Ctrl Pts',(-1.8693780394412,1.,-0.424678177290876));
#28290=CARTESIAN_POINT('Ctrl Pts',(-1.86408083333863,1.,-0.422327307417884));
#28291=CARTESIAN_POINT('Ctrl Pts',(-1.8590328109667,1.,-0.420157287975583));
#28292=CARTESIAN_POINT('Ctrl Pts',(-1.8541763285645,1.,-0.418164129144045));
#28293=CARTESIAN_POINT('Ctrl Pts',(-1.84929312930314,1.,-0.416300022039885));
#28294=CARTESIAN_POINT('Ctrl Pts',(-1.84405757074218,1.,-0.414487438255542));
#28295=CARTESIAN_POINT('Ctrl Pts',(-1.8380895347617,1.,-0.412633125322945));
#28296=CARTESIAN_POINT('Ctrl Pts',(-1.83100408895047,1.,-0.410641256301276));
#28297=CARTESIAN_POINT('Ctrl Pts',(-1.82247022677562,1.,-0.408428948106227));
#28298=CARTESIAN_POINT('Ctrl Pts',(-1.81223801812013,1.,-0.405933518407175));
#28299=CARTESIAN_POINT('Ctrl Pts',(-1.80012077173238,1.,-0.403107976163396));
#28300=CARTESIAN_POINT('Ctrl Pts',(-1.78598826343754,1.,-0.399919403774155));
#28301=CARTESIAN_POINT('Ctrl Pts',(-1.76975560043442,1.,-0.396346196110688));
#28302=CARTESIAN_POINT('Ctrl Pts',(-1.75137405310193,1.,-0.392375812285395));
#28303=CARTESIAN_POINT('Ctrl Pts',(-1.73493170972829,1.,-0.388877023502615));
#28304=CARTESIAN_POINT('Ctrl Pts',(-1.72162022244582,1.,-0.386070790323281));
#28305=CARTESIAN_POINT('Ctrl Pts',(-1.71231062891398,1.,-0.384119047314215));
#28306=CARTESIAN_POINT('Ctrl Pts',(-1.7075470150345,1.,-0.383122945602004));
#28307=CARTESIAN_POINT('',(-2.11275013067528,0.,-0.61342227326009));
#28308=CARTESIAN_POINT('Origin',(-2.0698113262342,0.,-0.745574324794401));
#28309=CARTESIAN_POINT('',(-2.0698113262342,1.,-0.745574324794401));
#28310=CARTESIAN_POINT('',(-2.11275013067528,1.,-0.61342227326009));
#28311=CARTESIAN_POINT('',(-2.0698113262342,0.,-0.745574324794401));
#28312=CARTESIAN_POINT('Ctrl Pts',(-1.60662857109684,-1.,-0.693717979106306));
#28313=CARTESIAN_POINT('Ctrl Pts',(-1.60662857109684,1.,-0.693717979106306));
#28314=CARTESIAN_POINT('Ctrl Pts',(-1.61106790958151,-1.,-0.695712097881194));
#28315=CARTESIAN_POINT('Ctrl Pts',(-1.61106790958151,1.,-0.695712097881194));
#28316=CARTESIAN_POINT('Ctrl Pts',(-1.61974673472612,-1.,-0.699605146405088));
#28317=CARTESIAN_POINT('Ctrl Pts',(-1.61974673472612,1.,-0.699605146405088));
#28318=CARTESIAN_POINT('Ctrl Pts',(-1.63216541664676,-1.,-0.705159151988319));
#28319=CARTESIAN_POINT('Ctrl Pts',(-1.63216541664676,1.,-0.705159151988319));
#28320=CARTESIAN_POINT('Ctrl Pts',(-1.64752408832016,-1.,-0.711993139355394));
#28321=CARTESIAN_POINT('Ctrl Pts',(-1.64752408832016,1.,-0.711993139355394));
#28322=CARTESIAN_POINT('Ctrl Pts',(-1.6647288055568,-1.,-0.719585433804282));
#28323=CARTESIAN_POINT('Ctrl Pts',(-1.6647288055568,1.,-0.719585433804282));
#28324=CARTESIAN_POINT('Ctrl Pts',(-1.67996158455503,-1.,-0.726235967997433));
#28325=CARTESIAN_POINT('Ctrl Pts',(-1.67996158455503,1.,-0.726235967997433));
#28326=CARTESIAN_POINT('Ctrl Pts',(-1.69326921975743,-1.,-0.731963238697195));
#28327=CARTESIAN_POINT('Ctrl Pts',(-1.69326921975743,1.,-0.731963238697195));
#28328=CARTESIAN_POINT('Ctrl Pts',(-1.70473309006121,-1.,-0.736799665724771));
#28329=CARTESIAN_POINT('Ctrl Pts',(-1.70473309006121,1.,-0.736799665724771));
#28330=CARTESIAN_POINT('Ctrl Pts',(-1.71447789751927,-1.,-0.740795162032087));
#28331=CARTESIAN_POINT('Ctrl Pts',(-1.71447789751927,1.,-0.740795162032087));
#28332=CARTESIAN_POINT('Ctrl Pts',(-1.7226822991693,-1.,-0.744021445433764));
#28333=CARTESIAN_POINT('Ctrl Pts',(-1.7226822991693,1.,-0.744021445433764));
#28334=CARTESIAN_POINT('Ctrl Pts',(-1.72958533647399,-1.,-0.746574710096436));
#28335=CARTESIAN_POINT('Ctrl Pts',(-1.72958533647399,1.,-0.746574710096436));
#28336=CARTESIAN_POINT('Ctrl Pts',(-1.73550351679848,-1.,-0.748582462954854));
#28337=CARTESIAN_POINT('Ctrl Pts',(-1.73550351679848,1.,-0.748582462954854));
#28338=CARTESIAN_POINT('Ctrl Pts',(-1.74080458266705,-1.,-0.75019343597954));
#28339=CARTESIAN_POINT('Ctrl Pts',(-1.74080458266705,1.,-0.75019343597954));
#28340=CARTESIAN_POINT('Ctrl Pts',(-1.74585086852298,-1.,-0.751555614163629));
#28341=CARTESIAN_POINT('Ctrl Pts',(-1.74585086852298,1.,-0.751555614163629));
#28342=CARTESIAN_POINT('Ctrl Pts',(-1.75095139468809,-1.,-0.752797683531377));
#28343=CARTESIAN_POINT('Ctrl Pts',(-1.75095139468809,1.,-0.752797683531377));
#28344=CARTESIAN_POINT('Ctrl Pts',(-1.75631083600175,-1.,-0.75400925402848));
#28345=CARTESIAN_POINT('Ctrl Pts',(-1.75631083600175,1.,-0.75400925402848));
#28346=CARTESIAN_POINT('Ctrl Pts',(-1.7619781724032,-1.,-0.755220979975262));
#28347=CARTESIAN_POINT('Ctrl Pts',(-1.7619781724032,1.,-0.755220979975262));
#28348=CARTESIAN_POINT('Ctrl Pts',(-1.76789396003141,-1.,-0.756421896028403));
#28349=CARTESIAN_POINT('Ctrl Pts',(-1.76789396003141,1.,-0.756421896028403));
#28350=CARTESIAN_POINT('Ctrl Pts',(-1.77394167108342,-1.,-0.757578264077238));
#28351=CARTESIAN_POINT('Ctrl Pts',(-1.77394167108342,1.,-0.757578264077238));
#28352=CARTESIAN_POINT('Ctrl Pts',(-1.77999411220912,-1.,-0.75865062667738));
#28353=CARTESIAN_POINT('Ctrl Pts',(-1.77999411220912,1.,-0.75865062667738));
#28354=CARTESIAN_POINT('Ctrl Pts',(-1.78596964884526,-1.,-0.759614401109868));
#28355=CARTESIAN_POINT('Ctrl Pts',(-1.78596964884526,1.,-0.759614401109868));
#28356=CARTESIAN_POINT('Ctrl Pts',(-1.79185815610802,-1.,-0.760469555880425));
#28357=CARTESIAN_POINT('Ctrl Pts',(-1.79185815610802,1.,-0.760469555880425));
#28358=CARTESIAN_POINT('Ctrl Pts',(-1.79768986997735,-1.,-0.761229695230359));
#28359=CARTESIAN_POINT('Ctrl Pts',(-1.79768986997735,1.,-0.761229695230359));
#28360=CARTESIAN_POINT('Ctrl Pts',(-1.80351583877334,-1.,-0.761915336443515));
#28361=CARTESIAN_POINT('Ctrl Pts',(-1.80351583877334,1.,-0.761915336443515));
#28362=CARTESIAN_POINT('Ctrl Pts',(-1.80938551463989,-1.,-0.762546129464036));
#28363=CARTESIAN_POINT('Ctrl Pts',(-1.80938551463989,1.,-0.762546129464036));
#28364=CARTESIAN_POINT('Ctrl Pts',(-1.81532118405566,-1.,-0.763132003836783));
#28365=CARTESIAN_POINT('Ctrl Pts',(-1.81532118405566,1.,-0.763132003836783));
#28366=CARTESIAN_POINT('Ctrl Pts',(-1.82131873145297,-1.,-0.763673465462854));
#28367=CARTESIAN_POINT('Ctrl Pts',(-1.82131873145297,1.,-0.763673465462854));
#28368=CARTESIAN_POINT('Ctrl Pts',(-1.8273599120008,-1.,-0.764165902606055));
#28369=CARTESIAN_POINT('Ctrl Pts',(-1.8273599120008,1.,-0.764165902606055));
#28370=CARTESIAN_POINT('Ctrl Pts',(-1.8334207722714,-1.,-0.764602549687845));
#28371=CARTESIAN_POINT('Ctrl Pts',(-1.8334207722714,1.,-0.764602549687845));
#28372=CARTESIAN_POINT('Ctrl Pts',(-1.83948181064823,-1.,-0.764978057881687));
#28373=CARTESIAN_POINT('Ctrl Pts',(-1.83948181064823,1.,-0.764978057881687));
#28374=CARTESIAN_POINT('Ctrl Pts',(-1.8455369887591,-1.,-0.765291664861971));
#28375=CARTESIAN_POINT('Ctrl Pts',(-1.8455369887591,1.,-0.765291664861971));
#28376=CARTESIAN_POINT('Ctrl Pts',(-1.85158945130054,-1.,-0.765545710619023));
#28377=CARTESIAN_POINT('Ctrl Pts',(-1.85158945130054,1.,-0.765545710619023));
#28378=CARTESIAN_POINT('Ctrl Pts',(-1.85764741390391,-1.,-0.765744212909305));
#28379=CARTESIAN_POINT('Ctrl Pts',(-1.85764741390391,1.,-0.765744212909305));
#28380=CARTESIAN_POINT('Ctrl Pts',(-1.86372027063314,-1.,-0.765891519092557));
#28381=CARTESIAN_POINT('Ctrl Pts',(-1.86372027063314,1.,-0.765891519092557));
#28382=CARTESIAN_POINT('Ctrl Pts',(-1.86981398314345,-1.,-0.765990708546111));
#28383=CARTESIAN_POINT('Ctrl Pts',(-1.86981398314345,1.,-0.765990708546111));
#28384=CARTESIAN_POINT('Ctrl Pts',(-1.87592888967886,-1.,-0.766042837036759));
#28385=CARTESIAN_POINT('Ctrl Pts',(-1.87592888967886,1.,-0.766042837036759));
#28386=CARTESIAN_POINT('Ctrl Pts',(-1.88206215302561,-1.,-0.766047794851868));
#28387=CARTESIAN_POINT('Ctrl Pts',(-1.88206215302561,1.,-0.766047794851868));
#28388=CARTESIAN_POINT('Ctrl Pts',(-1.88820926433409,-1.,-0.76600483706209));
#28389=CARTESIAN_POINT('Ctrl Pts',(-1.88820926433409,1.,-0.76600483706209));
#28390=CARTESIAN_POINT('Ctrl Pts',(-1.89436577771389,-1.,-0.765913193856979));
#28391=CARTESIAN_POINT('Ctrl Pts',(-1.89436577771389,1.,-0.765913193856979));
#28392=CARTESIAN_POINT('Ctrl Pts',(-1.90052930393599,-1.,-0.765772772593395));
#28393=CARTESIAN_POINT('Ctrl Pts',(-1.90052930393599,1.,-0.765772772593395));
#28394=CARTESIAN_POINT('Ctrl Pts',(-1.90669961402362,-1.,-0.765584196937936));
#28395=CARTESIAN_POINT('Ctrl Pts',(-1.90669961402362,1.,-0.765584196937936));
#28396=CARTESIAN_POINT('Ctrl Pts',(-1.91287765805174,-1.,-0.765348465884739));
#28397=CARTESIAN_POINT('Ctrl Pts',(-1.91287765805174,1.,-0.765348465884739));
#28398=CARTESIAN_POINT('Ctrl Pts',(-1.91906491634197,-1.,-0.765066729667095));
#28399=CARTESIAN_POINT('Ctrl Pts',(-1.91906491634197,1.,-0.765066729667095));
#28400=CARTESIAN_POINT('Ctrl Pts',(-1.92526263537041,-1.,-0.764740025488189));
#28401=CARTESIAN_POINT('Ctrl Pts',(-1.92526263537041,1.,-0.764740025488189));
#28402=CARTESIAN_POINT('Ctrl Pts',(-1.93147105496367,-1.,-0.764369010673889));
#28403=CARTESIAN_POINT('Ctrl Pts',(-1.93147105496367,1.,-0.764369010673889));
#28404=CARTESIAN_POINT('Ctrl Pts',(-1.93768964875867,-1.,-0.763954049121393));
#28405=CARTESIAN_POINT('Ctrl Pts',(-1.93768964875867,1.,-0.763954049121393));
#28406=CARTESIAN_POINT('Ctrl Pts',(-1.94391746617626,-1.,-0.76349533353858));
#28407=CARTESIAN_POINT('Ctrl Pts',(-1.94391746617626,1.,-0.76349533353858));
#28408=CARTESIAN_POINT('Ctrl Pts',(-1.95015342590025,-1.,-0.762992990878774));
#28409=CARTESIAN_POINT('Ctrl Pts',(-1.95015342590025,1.,-0.762992990878774));
#28410=CARTESIAN_POINT('Ctrl Pts',(-1.95639665309893,-1.,-0.762447203806263));
#28411=CARTESIAN_POINT('Ctrl Pts',(-1.95639665309893,1.,-0.762447203806263));
#28412=CARTESIAN_POINT('Ctrl Pts',(-1.96264672744229,-1.,-0.761858300014575));
#28413=CARTESIAN_POINT('Ctrl Pts',(-1.96264672744229,1.,-0.761858300014575));
#28414=CARTESIAN_POINT('Ctrl Pts',(-1.96890351582545,-1.,-0.761226690483986));
#28415=CARTESIAN_POINT('Ctrl Pts',(-1.96890351582545,1.,-0.761226690483986));
#28416=CARTESIAN_POINT('Ctrl Pts',(-1.97516705321521,-1.,-0.760552825409855));
#28417=CARTESIAN_POINT('Ctrl Pts',(-1.97516705321521,1.,-0.760552825409855));
#28418=CARTESIAN_POINT('Ctrl Pts',(-1.98143741418156,-1.,-0.759837147452135));
#28419=CARTESIAN_POINT('Ctrl Pts',(-1.98143741418156,1.,-0.759837147452135));
#28420=CARTESIAN_POINT('Ctrl Pts',(-1.98771456680806,-1.,-0.759080037802242));
#28421=CARTESIAN_POINT('Ctrl Pts',(-1.98771456680806,1.,-0.759080037802242));
#28422=CARTESIAN_POINT('Ctrl Pts',(-1.9939983109871,-1.,-0.758281796766377));
#28423=CARTESIAN_POINT('Ctrl Pts',(-1.9939983109871,1.,-0.758281796766377));
#28424=CARTESIAN_POINT('Ctrl Pts',(-2.00028834739072,-1.,-0.757442676862341));
#28425=CARTESIAN_POINT('Ctrl Pts',(-2.00028834739072,1.,-0.757442676862341));
#28426=CARTESIAN_POINT('Ctrl Pts',(-2.00658431587682,-1.,-0.756562904646496));
#28427=CARTESIAN_POINT('Ctrl Pts',(-2.00658431587682,1.,-0.756562904646496));
#28428=CARTESIAN_POINT('Ctrl Pts',(-2.01288584328149,-1.,-0.7556427049581));
#28429=CARTESIAN_POINT('Ctrl Pts',(-2.01288584328149,1.,-0.7556427049581));
#28430=CARTESIAN_POINT('Ctrl Pts',(-2.01919259406003,-1.,-0.75468233072352));
#28431=CARTESIAN_POINT('Ctrl Pts',(-2.01919259406003,1.,-0.75468233072352));
#28432=CARTESIAN_POINT('Ctrl Pts',(-2.02550428623587,-1.,-0.753682061113765));
#28433=CARTESIAN_POINT('Ctrl Pts',(-2.02550428623587,1.,-0.753682061113765));
#28434=CARTESIAN_POINT('Ctrl Pts',(-2.03182068456467,-1.,-0.752642180488104));
#28435=CARTESIAN_POINT('Ctrl Pts',(-2.03182068456467,1.,-0.752642180488104));
#28436=CARTESIAN_POINT('Ctrl Pts',(-2.03814160092173,-1.,-0.751562963361383));
#28437=CARTESIAN_POINT('Ctrl Pts',(-2.03814160092173,1.,-0.751562963361383));
#28438=CARTESIAN_POINT('Ctrl Pts',(-2.04446689147754,-1.,-0.750444657874758));
#28439=CARTESIAN_POINT('Ctrl Pts',(-2.04446689147754,1.,-0.750444657874758));
#28440=CARTESIAN_POINT('Ctrl Pts',(-2.05079645591606,-1.,-0.749287468663053));
#28441=CARTESIAN_POINT('Ctrl Pts',(-2.05079645591606,1.,-0.749287468663053));
#28442=CARTESIAN_POINT('Ctrl Pts',(-2.05713023030263,-1.,-0.748091554181101));
#28443=CARTESIAN_POINT('Ctrl Pts',(-2.05713023030263,1.,-0.748091554181101));
#28444=CARTESIAN_POINT('Ctrl Pts',(-2.06220058927162,-1.,-0.747103932785504));
#28445=CARTESIAN_POINT('Ctrl Pts',(-2.06220058927162,1.,-0.747103932785504));
#28446=CARTESIAN_POINT('Ctrl Pts',(-2.06600523016401,-1.,-0.746345871542695));
#28447=CARTESIAN_POINT('Ctrl Pts',(-2.06600523016401,1.,-0.746345871542695));
#28448=CARTESIAN_POINT('Ctrl Pts',(-2.06854248895575,-1.,-0.74583279137781));
#28449=CARTESIAN_POINT('Ctrl Pts',(-2.06854248895575,1.,-0.74583279137781));
#28450=CARTESIAN_POINT('Ctrl Pts',(-2.0698113262342,-1.,-0.745574324794401));
#28451=CARTESIAN_POINT('Ctrl Pts',(-2.0698113262342,1.,-0.745574324794401));
#28452=CARTESIAN_POINT('',(-1.60662857109684,1.,-0.693717979106306));
#28453=CARTESIAN_POINT('Ctrl Pts',(-1.60662857109684,1.,-0.693717979106306));
#28454=CARTESIAN_POINT('Ctrl Pts',(-1.61106790958151,1.,-0.695712097881194));
#28455=CARTESIAN_POINT('Ctrl Pts',(-1.61974673472612,1.,-0.699605146405088));
#28456=CARTESIAN_POINT('Ctrl Pts',(-1.63216541664676,1.,-0.705159151988319));
#28457=CARTESIAN_POINT('Ctrl Pts',(-1.64752408832016,1.,-0.711993139355394));
#28458=CARTESIAN_POINT('Ctrl Pts',(-1.6647288055568,1.,-0.719585433804282));
#28459=CARTESIAN_POINT('Ctrl Pts',(-1.67996158455503,1.,-0.726235967997433));
#28460=CARTESIAN_POINT('Ctrl Pts',(-1.69326921975743,1.,-0.731963238697195));
#28461=CARTESIAN_POINT('Ctrl Pts',(-1.70473309006121,1.,-0.736799665724771));
#28462=CARTESIAN_POINT('Ctrl Pts',(-1.71447789751927,1.,-0.740795162032087));
#28463=CARTESIAN_POINT('Ctrl Pts',(-1.7226822991693,1.,-0.744021445433764));
#28464=CARTESIAN_POINT('Ctrl Pts',(-1.72958533647399,1.,-0.746574710096436));
#28465=CARTESIAN_POINT('Ctrl Pts',(-1.73550351679848,1.,-0.748582462954854));
#28466=CARTESIAN_POINT('Ctrl Pts',(-1.74080458266705,1.,-0.75019343597954));
#28467=CARTESIAN_POINT('Ctrl Pts',(-1.74585086852298,1.,-0.751555614163629));
#28468=CARTESIAN_POINT('Ctrl Pts',(-1.75095139468809,1.,-0.752797683531377));
#28469=CARTESIAN_POINT('Ctrl Pts',(-1.75631083600175,1.,-0.75400925402848));
#28470=CARTESIAN_POINT('Ctrl Pts',(-1.7619781724032,1.,-0.755220979975262));
#28471=CARTESIAN_POINT('Ctrl Pts',(-1.76789396003141,1.,-0.756421896028403));
#28472=CARTESIAN_POINT('Ctrl Pts',(-1.77394167108342,1.,-0.757578264077238));
#28473=CARTESIAN_POINT('Ctrl Pts',(-1.77999411220912,1.,-0.75865062667738));
#28474=CARTESIAN_POINT('Ctrl Pts',(-1.78596964884526,1.,-0.759614401109868));
#28475=CARTESIAN_POINT('Ctrl Pts',(-1.79185815610802,1.,-0.760469555880425));
#28476=CARTESIAN_POINT('Ctrl Pts',(-1.79768986997735,1.,-0.761229695230359));
#28477=CARTESIAN_POINT('Ctrl Pts',(-1.80351583877334,1.,-0.761915336443515));
#28478=CARTESIAN_POINT('Ctrl Pts',(-1.80938551463989,1.,-0.762546129464036));
#28479=CARTESIAN_POINT('Ctrl Pts',(-1.81532118405566,1.,-0.763132003836783));
#28480=CARTESIAN_POINT('Ctrl Pts',(-1.82131873145297,1.,-0.763673465462854));
#28481=CARTESIAN_POINT('Ctrl Pts',(-1.8273599120008,1.,-0.764165902606055));
#28482=CARTESIAN_POINT('Ctrl Pts',(-1.8334207722714,1.,-0.764602549687845));
#28483=CARTESIAN_POINT('Ctrl Pts',(-1.83948181064823,1.,-0.764978057881687));
#28484=CARTESIAN_POINT('Ctrl Pts',(-1.8455369887591,1.,-0.765291664861971));
#28485=CARTESIAN_POINT('Ctrl Pts',(-1.85158945130054,1.,-0.765545710619023));
#28486=CARTESIAN_POINT('Ctrl Pts',(-1.85764741390391,1.,-0.765744212909305));
#28487=CARTESIAN_POINT('Ctrl Pts',(-1.86372027063314,1.,-0.765891519092557));
#28488=CARTESIAN_POINT('Ctrl Pts',(-1.86981398314345,1.,-0.765990708546111));
#28489=CARTESIAN_POINT('Ctrl Pts',(-1.87592888967886,1.,-0.766042837036759));
#28490=CARTESIAN_POINT('Ctrl Pts',(-1.88206215302561,1.,-0.766047794851868));
#28491=CARTESIAN_POINT('Ctrl Pts',(-1.88820926433409,1.,-0.76600483706209));
#28492=CARTESIAN_POINT('Ctrl Pts',(-1.89436577771389,1.,-0.765913193856979));
#28493=CARTESIAN_POINT('Ctrl Pts',(-1.90052930393599,1.,-0.765772772593395));
#28494=CARTESIAN_POINT('Ctrl Pts',(-1.90669961402362,1.,-0.765584196937936));
#28495=CARTESIAN_POINT('Ctrl Pts',(-1.91287765805174,1.,-0.765348465884739));
#28496=CARTESIAN_POINT('Ctrl Pts',(-1.91906491634197,1.,-0.765066729667095));
#28497=CARTESIAN_POINT('Ctrl Pts',(-1.92526263537041,1.,-0.764740025488189));
#28498=CARTESIAN_POINT('Ctrl Pts',(-1.93147105496367,1.,-0.764369010673889));
#28499=CARTESIAN_POINT('Ctrl Pts',(-1.93768964875867,1.,-0.763954049121393));
#28500=CARTESIAN_POINT('Ctrl Pts',(-1.94391746617626,1.,-0.76349533353858));
#28501=CARTESIAN_POINT('Ctrl Pts',(-1.95015342590025,1.,-0.762992990878774));
#28502=CARTESIAN_POINT('Ctrl Pts',(-1.95639665309893,1.,-0.762447203806263));
#28503=CARTESIAN_POINT('Ctrl Pts',(-1.96264672744229,1.,-0.761858300014575));
#28504=CARTESIAN_POINT('Ctrl Pts',(-1.96890351582545,1.,-0.761226690483986));
#28505=CARTESIAN_POINT('Ctrl Pts',(-1.97516705321521,1.,-0.760552825409855));
#28506=CARTESIAN_POINT('Ctrl Pts',(-1.98143741418156,1.,-0.759837147452135));
#28507=CARTESIAN_POINT('Ctrl Pts',(-1.98771456680806,1.,-0.759080037802242));
#28508=CARTESIAN_POINT('Ctrl Pts',(-1.9939983109871,1.,-0.758281796766377));
#28509=CARTESIAN_POINT('Ctrl Pts',(-2.00028834739072,1.,-0.757442676862341));
#28510=CARTESIAN_POINT('Ctrl Pts',(-2.00658431587682,1.,-0.756562904646496));
#28511=CARTESIAN_POINT('Ctrl Pts',(-2.01288584328149,1.,-0.7556427049581));
#28512=CARTESIAN_POINT('Ctrl Pts',(-2.01919259406003,1.,-0.75468233072352));
#28513=CARTESIAN_POINT('Ctrl Pts',(-2.02550428623587,1.,-0.753682061113765));
#28514=CARTESIAN_POINT('Ctrl Pts',(-2.03182068456467,1.,-0.752642180488104));
#28515=CARTESIAN_POINT('Ctrl Pts',(-2.03814160092173,1.,-0.751562963361383));
#28516=CARTESIAN_POINT('Ctrl Pts',(-2.04446689147754,1.,-0.750444657874758));
#28517=CARTESIAN_POINT('Ctrl Pts',(-2.05079645591606,1.,-0.749287468663053));
#28518=CARTESIAN_POINT('Ctrl Pts',(-2.05713023030263,1.,-0.748091554181101));
#28519=CARTESIAN_POINT('Ctrl Pts',(-2.06220058927162,1.,-0.747103932785504));
#28520=CARTESIAN_POINT('Ctrl Pts',(-2.06600523016401,1.,-0.746345871542695));
#28521=CARTESIAN_POINT('Ctrl Pts',(-2.06854248895575,1.,-0.74583279137781));
#28522=CARTESIAN_POINT('Ctrl Pts',(-2.0698113262342,1.,-0.745574324794401));
#28523=CARTESIAN_POINT('',(-1.60662857109684,0.,-0.693717979106306));
#28524=CARTESIAN_POINT('Origin',(0.,0.,0.));
#28525=CARTESIAN_POINT('',(-1.5055822144029,1.,-0.892032620296855));
#28526=CARTESIAN_POINT('Origin',(0.,1.,0.));
#28527=CARTESIAN_POINT('',(-1.5055822144029,0.,-0.892032620296855));
#28528=CARTESIAN_POINT('Ctrl Pts',(-1.81978687191668,-1.,-1.23627494547115));
#28529=CARTESIAN_POINT('Ctrl Pts',(-1.81978687191668,1.,-1.23627494547115));
#28530=CARTESIAN_POINT('Ctrl Pts',(-1.81925017193666,-1.,-1.23509651170476));
#28531=CARTESIAN_POINT('Ctrl Pts',(-1.81925017193666,1.,-1.23509651170476));
#28532=CARTESIAN_POINT('Ctrl Pts',(-1.81817389921279,-1.,-1.2327422452705));
#28533=CARTESIAN_POINT('Ctrl Pts',(-1.81817389921279,1.,-1.2327422452705));
#28534=CARTESIAN_POINT('Ctrl Pts',(-1.8165508718364,-1.,-1.2292186489137));
#28535=CARTESIAN_POINT('Ctrl Pts',(-1.8165508718364,1.,-1.2292186489137));
#28536=CARTESIAN_POINT('Ctrl Pts',(-1.81436959210434,-1.,-1.2245361330495));
#28537=CARTESIAN_POINT('Ctrl Pts',(-1.81436959210434,1.,-1.2245361330495));
#28538=CARTESIAN_POINT('Ctrl Pts',(-1.81161420806656,-1.,-1.21870906103557));
#28539=CARTESIAN_POINT('Ctrl Pts',(-1.81161420806656,1.,-1.21870906103557));
#28540=CARTESIAN_POINT('Ctrl Pts',(-1.80882996917129,-1.,-1.21290815708314));
#28541=CARTESIAN_POINT('Ctrl Pts',(-1.80882996917129,1.,-1.21290815708314));
#28542=CARTESIAN_POINT('Ctrl Pts',(-1.80601678480707,-1.,-1.20713356605475));
#28543=CARTESIAN_POINT('Ctrl Pts',(-1.80601678480707,1.,-1.20713356605475));
#28544=CARTESIAN_POINT('Ctrl Pts',(-1.80317454838603,-1.,-1.20138548938974));
#28545=CARTESIAN_POINT('Ctrl Pts',(-1.80317454838603,1.,-1.20138548938974));
#28546=CARTESIAN_POINT('Ctrl Pts',(-1.80030314369879,-1.,-1.19566418930242));
#28547=CARTESIAN_POINT('Ctrl Pts',(-1.80030314369879,1.,-1.19566418930242));
#28548=CARTESIAN_POINT('Ctrl Pts',(-1.79740245923478,-1.,-1.18996997934445));
#28549=CARTESIAN_POINT('Ctrl Pts',(-1.79740245923478,1.,-1.18996997934445));
#28550=CARTESIAN_POINT('Ctrl Pts',(-1.79447240321515,-1.,-1.18430321697432));
#28551=CARTESIAN_POINT('Ctrl Pts',(-1.79447240321515,1.,-1.18430321697432));
#28552=CARTESIAN_POINT('Ctrl Pts',(-1.79151291552689,-1.,-1.17866429440809));
#28553=CARTESIAN_POINT('Ctrl Pts',(-1.79151291552689,1.,-1.17866429440809));
#28554=CARTESIAN_POINT('Ctrl Pts',(-1.78852398877616,-1.,-1.17305363177328));
#28555=CARTESIAN_POINT('Ctrl Pts',(-1.78852398877616,1.,-1.17305363177328));
#28556=CARTESIAN_POINT('Ctrl Pts',(-1.78550566040443,-1.,-1.16747166312303));
#28557=CARTESIAN_POINT('Ctrl Pts',(-1.78550566040443,1.,-1.16747166312303));
#28558=CARTESIAN_POINT('Ctrl Pts',(-1.78245795881009,-1.,-1.16191881298499));
#28559=CARTESIAN_POINT('Ctrl Pts',(-1.78245795881009,1.,-1.16191881298499));
#28560=CARTESIAN_POINT('Ctrl Pts',(-1.77938085564275,-1.,-1.15639547194698));
#28561=CARTESIAN_POINT('Ctrl Pts',(-1.77938085564275,1.,-1.15639547194698));
#28562=CARTESIAN_POINT('Ctrl Pts',(-1.7762742255701,-1.,-1.15090197841515));
#28563=CARTESIAN_POINT('Ctrl Pts',(-1.7762742255701,1.,-1.15090197841515));
#28564=CARTESIAN_POINT('Ctrl Pts',(-1.77313777896194,-1.,-1.1454385822692));
#28565=CARTESIAN_POINT('Ctrl Pts',(-1.77313777896194,1.,-1.1454385822692));
#28566=CARTESIAN_POINT('Ctrl Pts',(-1.76997111386769,-1.,-1.14000548336975));
#28567=CARTESIAN_POINT('Ctrl Pts',(-1.76997111386769,1.,-1.14000548336975));
#28568=CARTESIAN_POINT('Ctrl Pts',(-1.76677384551862,-1.,-1.1346029180462));
#28569=CARTESIAN_POINT('Ctrl Pts',(-1.76677384551862,1.,-1.1346029180462));
#28570=CARTESIAN_POINT('Ctrl Pts',(-1.7635457196617,-1.,-1.12923123555075));
#28571=CARTESIAN_POINT('Ctrl Pts',(-1.7635457196617,1.,-1.12923123555075));
#28572=CARTESIAN_POINT('Ctrl Pts',(-1.76028671825096,-1.,-1.12389096855086));
#28573=CARTESIAN_POINT('Ctrl Pts',(-1.76028671825096,1.,-1.12389096855086));
#28574=CARTESIAN_POINT('Ctrl Pts',(-1.75699720772105,-1.,-1.11858293216763));
#28575=CARTESIAN_POINT('Ctrl Pts',(-1.75699720772105,1.,-1.11858293216763));
#28576=CARTESIAN_POINT('Ctrl Pts',(-1.7536777209463,-1.,-1.11330807582551));
#28577=CARTESIAN_POINT('Ctrl Pts',(-1.7536777209463,1.,-1.11330807582551));
#28578=CARTESIAN_POINT('Ctrl Pts',(-1.7503286607592,-1.,-1.10806728183007));
#28579=CARTESIAN_POINT('Ctrl Pts',(-1.7503286607592,1.,-1.10806728183007));
#28580=CARTESIAN_POINT('Ctrl Pts',(-1.74695004214923,-1.,-1.10286118991143));
#28581=CARTESIAN_POINT('Ctrl Pts',(-1.74695004214923,1.,-1.10286118991143));
#28582=CARTESIAN_POINT('Ctrl Pts',(-1.74354119236208,-1.,-1.09768999241225));
#28583=CARTESIAN_POINT('Ctrl Pts',(-1.74354119236208,1.,-1.09768999241225));
#28584=CARTESIAN_POINT('Ctrl Pts',(-1.74010053962247,-1.,-1.09255329056493));
#28585=CARTESIAN_POINT('Ctrl Pts',(-1.74010053962247,1.,-1.09255329056493));
#28586=CARTESIAN_POINT('Ctrl Pts',(-1.73662628326091,-1.,-1.08745056285427));
#28587=CARTESIAN_POINT('Ctrl Pts',(-1.73662628326091,1.,-1.08745056285427));
#28588=CARTESIAN_POINT('Ctrl Pts',(-1.73311705663407,-1.,-1.08238162784749));
#28589=CARTESIAN_POINT('Ctrl Pts',(-1.73311705663407,1.,-1.08238162784749));
#28590=CARTESIAN_POINT('Ctrl Pts',(-1.72957248977424,-1.,-1.0773470373727));
#28591=CARTESIAN_POINT('Ctrl Pts',(-1.72957248977424,1.,-1.0773470373727));
#28592=CARTESIAN_POINT('Ctrl Pts',(-1.72599406198488,-1.,-1.07234866990252));
#28593=CARTESIAN_POINT('Ctrl Pts',(-1.72599406198488,1.,-1.07234866990252));
#28594=CARTESIAN_POINT('Ctrl Pts',(-1.72238500928453,-1.,-1.06738966975462));
#28595=CARTESIAN_POINT('Ctrl Pts',(-1.72238500928453,1.,-1.06738966975462));
#28596=CARTESIAN_POINT('Ctrl Pts',(-1.71874858456904,-1.,-1.06247324680647));
#28597=CARTESIAN_POINT('Ctrl Pts',(-1.71874858456904,1.,-1.06247324680647));
#28598=CARTESIAN_POINT('Ctrl Pts',(-1.7150865442702,-1.,-1.05760163192479));
#28599=CARTESIAN_POINT('Ctrl Pts',(-1.7150865442702,1.,-1.05760163192479));
#28600=CARTESIAN_POINT('Ctrl Pts',(-1.71139783543989,-1.,-1.05277517202855));
#28601=CARTESIAN_POINT('Ctrl Pts',(-1.71139783543989,1.,-1.05277517202855));
#28602=CARTESIAN_POINT('Ctrl Pts',(-1.70767646263649,-1.,-1.04799085404995));
#28603=CARTESIAN_POINT('Ctrl Pts',(-1.70767646263649,1.,-1.04799085404995));
#28604=CARTESIAN_POINT('Ctrl Pts',(-1.70391338707982,-1.,-1.04324363334554));
#28605=CARTESIAN_POINT('Ctrl Pts',(-1.70391338707982,1.,-1.04324363334554));
#28606=CARTESIAN_POINT('Ctrl Pts',(-1.70010052930962,-1.,-1.03852922490789));
#28607=CARTESIAN_POINT('Ctrl Pts',(-1.70010052930962,1.,-1.03852922490789));
#28608=CARTESIAN_POINT('Ctrl Pts',(-1.69623414782771,-1.,-1.03384646003588));
#28609=CARTESIAN_POINT('Ctrl Pts',(-1.69623414782771,1.,-1.03384646003588));
#28610=CARTESIAN_POINT('Ctrl Pts',(-1.69231840863458,-1.,-1.02919977579147));
#28611=CARTESIAN_POINT('Ctrl Pts',(-1.69231840863458,1.,-1.02919977579147));
#28612=CARTESIAN_POINT('Ctrl Pts',(-1.68836910178447,-1.,-1.02460180535255));
#28613=CARTESIAN_POINT('Ctrl Pts',(-1.68836910178447,1.,-1.02460180535255));
#28614=CARTESIAN_POINT('Ctrl Pts',(-1.68440578021706,-1.,-1.02006795074201));
#28615=CARTESIAN_POINT('Ctrl Pts',(-1.68440578021706,1.,-1.02006795074201));
#28616=CARTESIAN_POINT('Ctrl Pts',(-1.68044289894798,-1.,-1.01561026162773));
#28617=CARTESIAN_POINT('Ctrl Pts',(-1.68044289894798,1.,-1.01561026162773));
#28618=CARTESIAN_POINT('Ctrl Pts',(-1.67648246776464,-1.,-1.01123236493511));
#28619=CARTESIAN_POINT('Ctrl Pts',(-1.67648246776464,1.,-1.01123236493511));
#28620=CARTESIAN_POINT('Ctrl Pts',(-1.67250335383293,-1.,-1.00692206696414));
#28621=CARTESIAN_POINT('Ctrl Pts',(-1.67250335383293,1.,-1.00692206696414));
#28622=CARTESIAN_POINT('Ctrl Pts',(-1.66846059277303,-1.,-1.00265091003727));
#28623=CARTESIAN_POINT('Ctrl Pts',(-1.66846059277303,1.,-1.00265091003727));
#28624=CARTESIAN_POINT('Ctrl Pts',(-1.66430758030376,-1.,-0.998389654952758));
#28625=CARTESIAN_POINT('Ctrl Pts',(-1.66430758030376,1.,-0.998389654952758));
#28626=CARTESIAN_POINT('Ctrl Pts',(-1.66001553809947,-1.,-0.994121836661306));
#28627=CARTESIAN_POINT('Ctrl Pts',(-1.66001553809947,1.,-0.994121836661306));
#28628=CARTESIAN_POINT('Ctrl Pts',(-1.65559044289699,-1.,-0.989855627854165));
#28629=CARTESIAN_POINT('Ctrl Pts',(-1.65559044289699,1.,-0.989855627854165));
#28630=CARTESIAN_POINT('Ctrl Pts',(-1.65110016612638,-1.,-0.985642622920821));
#28631=CARTESIAN_POINT('Ctrl Pts',(-1.65110016612638,1.,-0.985642622920821));
#28632=CARTESIAN_POINT('Ctrl Pts',(-1.64665139190656,-1.,-0.981562530939489));
#28633=CARTESIAN_POINT('Ctrl Pts',(-1.64665139190656,1.,-0.981562530939489));
#28634=CARTESIAN_POINT('Ctrl Pts',(-1.64233990826687,-1.,-0.977689794119416));
#28635=CARTESIAN_POINT('Ctrl Pts',(-1.64233990826687,1.,-0.977689794119416));
#28636=CARTESIAN_POINT('Ctrl Pts',(-1.63820952658144,-1.,-0.974066058287418));
#28637=CARTESIAN_POINT('Ctrl Pts',(-1.63820952658144,1.,-0.974066058287418));
#28638=CARTESIAN_POINT('Ctrl Pts',(-1.63420665729798,-1.,-0.970669715997509));
#28639=CARTESIAN_POINT('Ctrl Pts',(-1.63420665729798,1.,-0.970669715997509));
#28640=CARTESIAN_POINT('Ctrl Pts',(-1.63013849959461,-1.,-0.967387853230345));
#28641=CARTESIAN_POINT('Ctrl Pts',(-1.63013849959461,1.,-0.967387853230345));
#28642=CARTESIAN_POINT('Ctrl Pts',(-1.62571930670187,-1.,-0.964046107040536));
#28643=CARTESIAN_POINT('Ctrl Pts',(-1.62571930670187,1.,-0.964046107040536));
#28644=CARTESIAN_POINT('Ctrl Pts',(-1.62061638140221,-1.,-0.960438326101729));
#28645=CARTESIAN_POINT('Ctrl Pts',(-1.62061638140221,1.,-0.960438326101729));
#28646=CARTESIAN_POINT('Ctrl Pts',(-1.61449324337085,-1.,-0.956354422920671));
#28647=CARTESIAN_POINT('Ctrl Pts',(-1.61449324337085,1.,-0.956354422920671));
#28648=CARTESIAN_POINT('Ctrl Pts',(-1.60706069896936,-1.,-0.951613284356035));
#28649=CARTESIAN_POINT('Ctrl Pts',(-1.60706069896936,1.,-0.951613284356035));
#28650=CARTESIAN_POINT('Ctrl Pts',(-1.59810042043673,-1.,-0.946078063315257));
#28651=CARTESIAN_POINT('Ctrl Pts',(-1.59810042043673,1.,-0.946078063315257));
#28652=CARTESIAN_POINT('Ctrl Pts',(-1.58744937487176,-1.,-0.939646377893399));
#28653=CARTESIAN_POINT('Ctrl Pts',(-1.58744937487176,1.,-0.939646377893399));
#28654=CARTESIAN_POINT('Ctrl Pts',(-1.57499388382243,-1.,-0.932246680108685));
#28655=CARTESIAN_POINT('Ctrl Pts',(-1.57499388382243,1.,-0.932246680108685));
#28656=CARTESIAN_POINT('Ctrl Pts',(-1.56065988578893,-1.,-0.923832188944341));
#28657=CARTESIAN_POINT('Ctrl Pts',(-1.56065988578893,1.,-0.923832188944341));
#28658=CARTESIAN_POINT('Ctrl Pts',(-1.54440491149498,-1.,-0.914375919026456));
#28659=CARTESIAN_POINT('Ctrl Pts',(-1.54440491149498,1.,-0.914375919026456));
#28660=CARTESIAN_POINT('Ctrl Pts',(-1.52984849887993,-1.,-0.905967409625651));
#28661=CARTESIAN_POINT('Ctrl Pts',(-1.52984849887993,1.,-0.905967409625651));
#28662=CARTESIAN_POINT('Ctrl Pts',(-1.51805569590094,-1.,-0.899185047483511));
#28663=CARTESIAN_POINT('Ctrl Pts',(-1.51805569590094,1.,-0.899185047483511));
#28664=CARTESIAN_POINT('Ctrl Pts',(-1.50980486806688,-1.,-0.894452006964543));
#28665=CARTESIAN_POINT('Ctrl Pts',(-1.50980486806688,1.,-0.894452006964543));
#28666=CARTESIAN_POINT('Ctrl Pts',(-1.5055822144029,-1.,-0.892032620296855));
#28667=CARTESIAN_POINT('Ctrl Pts',(-1.5055822144029,1.,-0.892032620296855));
#28668=CARTESIAN_POINT('',(-1.81978687191668,1.,-1.23627494547115));
#28669=CARTESIAN_POINT('Ctrl Pts',(-1.81978687191668,1.,-1.23627494547115));
#28670=CARTESIAN_POINT('Ctrl Pts',(-1.81925017193666,1.,-1.23509651170476));
#28671=CARTESIAN_POINT('Ctrl Pts',(-1.81817389921279,1.,-1.2327422452705));
#28672=CARTESIAN_POINT('Ctrl Pts',(-1.8165508718364,1.,-1.2292186489137));
#28673=CARTESIAN_POINT('Ctrl Pts',(-1.81436959210434,1.,-1.2245361330495));
#28674=CARTESIAN_POINT('Ctrl Pts',(-1.81161420806656,1.,-1.21870906103557));
#28675=CARTESIAN_POINT('Ctrl Pts',(-1.80882996917129,1.,-1.21290815708314));
#28676=CARTESIAN_POINT('Ctrl Pts',(-1.80601678480707,1.,-1.20713356605475));
#28677=CARTESIAN_POINT('Ctrl Pts',(-1.80317454838603,1.,-1.20138548938974));
#28678=CARTESIAN_POINT('Ctrl Pts',(-1.80030314369879,1.,-1.19566418930242));
#28679=CARTESIAN_POINT('Ctrl Pts',(-1.79740245923478,1.,-1.18996997934445));
#28680=CARTESIAN_POINT('Ctrl Pts',(-1.79447240321515,1.,-1.18430321697432));
#28681=CARTESIAN_POINT('Ctrl Pts',(-1.79151291552689,1.,-1.17866429440809));
#28682=CARTESIAN_POINT('Ctrl Pts',(-1.78852398877616,1.,-1.17305363177328));
#28683=CARTESIAN_POINT('Ctrl Pts',(-1.78550566040443,1.,-1.16747166312303));
#28684=CARTESIAN_POINT('Ctrl Pts',(-1.78245795881009,1.,-1.16191881298499));
#28685=CARTESIAN_POINT('Ctrl Pts',(-1.77938085564275,1.,-1.15639547194698));
#28686=CARTESIAN_POINT('Ctrl Pts',(-1.7762742255701,1.,-1.15090197841515));
#28687=CARTESIAN_POINT('Ctrl Pts',(-1.77313777896194,1.,-1.1454385822692));
#28688=CARTESIAN_POINT('Ctrl Pts',(-1.76997111386769,1.,-1.14000548336975));
#28689=CARTESIAN_POINT('Ctrl Pts',(-1.76677384551862,1.,-1.1346029180462));
#28690=CARTESIAN_POINT('Ctrl Pts',(-1.7635457196617,1.,-1.12923123555075));
#28691=CARTESIAN_POINT('Ctrl Pts',(-1.76028671825096,1.,-1.12389096855086));
#28692=CARTESIAN_POINT('Ctrl Pts',(-1.75699720772105,1.,-1.11858293216763));
#28693=CARTESIAN_POINT('Ctrl Pts',(-1.7536777209463,1.,-1.11330807582551));
#28694=CARTESIAN_POINT('Ctrl Pts',(-1.7503286607592,1.,-1.10806728183007));
#28695=CARTESIAN_POINT('Ctrl Pts',(-1.74695004214923,1.,-1.10286118991143));
#28696=CARTESIAN_POINT('Ctrl Pts',(-1.74354119236208,1.,-1.09768999241225));
#28697=CARTESIAN_POINT('Ctrl Pts',(-1.74010053962247,1.,-1.09255329056493));
#28698=CARTESIAN_POINT('Ctrl Pts',(-1.73662628326091,1.,-1.08745056285427));
#28699=CARTESIAN_POINT('Ctrl Pts',(-1.73311705663407,1.,-1.08238162784749));
#28700=CARTESIAN_POINT('Ctrl Pts',(-1.72957248977424,1.,-1.0773470373727));
#28701=CARTESIAN_POINT('Ctrl Pts',(-1.72599406198488,1.,-1.07234866990252));
#28702=CARTESIAN_POINT('Ctrl Pts',(-1.72238500928453,1.,-1.06738966975462));
#28703=CARTESIAN_POINT('Ctrl Pts',(-1.71874858456904,1.,-1.06247324680647));
#28704=CARTESIAN_POINT('Ctrl Pts',(-1.7150865442702,1.,-1.05760163192479));
#28705=CARTESIAN_POINT('Ctrl Pts',(-1.71139783543989,1.,-1.05277517202855));
#28706=CARTESIAN_POINT('Ctrl Pts',(-1.70767646263649,1.,-1.04799085404995));
#28707=CARTESIAN_POINT('Ctrl Pts',(-1.70391338707982,1.,-1.04324363334554));
#28708=CARTESIAN_POINT('Ctrl Pts',(-1.70010052930962,1.,-1.03852922490789));
#28709=CARTESIAN_POINT('Ctrl Pts',(-1.69623414782771,1.,-1.03384646003588));
#28710=CARTESIAN_POINT('Ctrl Pts',(-1.69231840863458,1.,-1.02919977579147));
#28711=CARTESIAN_POINT('Ctrl Pts',(-1.68836910178447,1.,-1.02460180535255));
#28712=CARTESIAN_POINT('Ctrl Pts',(-1.68440578021706,1.,-1.02006795074201));
#28713=CARTESIAN_POINT('Ctrl Pts',(-1.68044289894798,1.,-1.01561026162773));
#28714=CARTESIAN_POINT('Ctrl Pts',(-1.67648246776464,1.,-1.01123236493511));
#28715=CARTESIAN_POINT('Ctrl Pts',(-1.67250335383293,1.,-1.00692206696414));
#28716=CARTESIAN_POINT('Ctrl Pts',(-1.66846059277303,1.,-1.00265091003727));
#28717=CARTESIAN_POINT('Ctrl Pts',(-1.66430758030376,1.,-0.998389654952758));
#28718=CARTESIAN_POINT('Ctrl Pts',(-1.66001553809947,1.,-0.994121836661306));
#28719=CARTESIAN_POINT('Ctrl Pts',(-1.65559044289699,1.,-0.989855627854165));
#28720=CARTESIAN_POINT('Ctrl Pts',(-1.65110016612638,1.,-0.985642622920821));
#28721=CARTESIAN_POINT('Ctrl Pts',(-1.64665139190656,1.,-0.981562530939489));
#28722=CARTESIAN_POINT('Ctrl Pts',(-1.64233990826687,1.,-0.977689794119416));
#28723=CARTESIAN_POINT('Ctrl Pts',(-1.63820952658144,1.,-0.974066058287418));
#28724=CARTESIAN_POINT('Ctrl Pts',(-1.63420665729798,1.,-0.970669715997509));
#28725=CARTESIAN_POINT('Ctrl Pts',(-1.63013849959461,1.,-0.967387853230345));
#28726=CARTESIAN_POINT('Ctrl Pts',(-1.62571930670187,1.,-0.964046107040536));
#28727=CARTESIAN_POINT('Ctrl Pts',(-1.62061638140221,1.,-0.960438326101729));
#28728=CARTESIAN_POINT('Ctrl Pts',(-1.61449324337085,1.,-0.956354422920671));
#28729=CARTESIAN_POINT('Ctrl Pts',(-1.60706069896936,1.,-0.951613284356035));
#28730=CARTESIAN_POINT('Ctrl Pts',(-1.59810042043673,1.,-0.946078063315257));
#28731=CARTESIAN_POINT('Ctrl Pts',(-1.58744937487176,1.,-0.939646377893399));
#28732=CARTESIAN_POINT('Ctrl Pts',(-1.57499388382243,1.,-0.932246680108685));
#28733=CARTESIAN_POINT('Ctrl Pts',(-1.56065988578893,1.,-0.923832188944341));
#28734=CARTESIAN_POINT('Ctrl Pts',(-1.54440491149498,1.,-0.914375919026456));
#28735=CARTESIAN_POINT('Ctrl Pts',(-1.52984849887993,1.,-0.905967409625651));
#28736=CARTESIAN_POINT('Ctrl Pts',(-1.51805569590094,1.,-0.899185047483511));
#28737=CARTESIAN_POINT('Ctrl Pts',(-1.50980486806688,1.,-0.894452006964543));
#28738=CARTESIAN_POINT('Ctrl Pts',(-1.5055822144029,1.,-0.892032620296855));
#28739=CARTESIAN_POINT('',(-1.81978687191668,0.,-1.23627494547115));
#28740=CARTESIAN_POINT('Origin',(-1.73811241238545,0.,-1.34869019493419));
#28741=CARTESIAN_POINT('',(-1.73811241238545,1.,-1.34869019493419));
#28742=CARTESIAN_POINT('',(-1.81978687191668,1.,-1.23627494547115));
#28743=CARTESIAN_POINT('',(-1.73811241238545,0.,-1.34869019493419));
#28744=CARTESIAN_POINT('Ctrl Pts',(-1.31362392696032,-1.,-1.15624053661742));
#28745=CARTESIAN_POINT('Ctrl Pts',(-1.31362392696032,1.,-1.15624053661742));
#28746=CARTESIAN_POINT('Ctrl Pts',(-1.31722977216397,-1.,-1.15950888730809));
#28747=CARTESIAN_POINT('Ctrl Pts',(-1.31722977216397,1.,-1.15950888730809));
#28748=CARTESIAN_POINT('Ctrl Pts',(-1.32428080721772,-1.,-1.16589330093588));
#28749=CARTESIAN_POINT('Ctrl Pts',(-1.32428080721772,1.,-1.16589330093588));
#28750=CARTESIAN_POINT('Ctrl Pts',(-1.33437539347008,-1.,-1.17501305789857));
#28751=CARTESIAN_POINT('Ctrl Pts',(-1.33437539347008,1.,-1.17501305789857));
#28752=CARTESIAN_POINT('Ctrl Pts',(-1.34687054001093,-1.,-1.18625865667441));
#28753=CARTESIAN_POINT('Ctrl Pts',(-1.34687054001093,1.,-1.18625865667441));
#28754=CARTESIAN_POINT('Ctrl Pts',(-1.36088705043885,-1.,-1.1987959077932));
#28755=CARTESIAN_POINT('Ctrl Pts',(-1.36088705043885,1.,-1.1987959077932));
#28756=CARTESIAN_POINT('Ctrl Pts',(-1.37331915607905,-1.,-1.20982812925645));
#28757=CARTESIAN_POINT('Ctrl Pts',(-1.37331915607905,1.,-1.20982812925645));
#28758=CARTESIAN_POINT('Ctrl Pts',(-1.38420564527715,-1.,-1.21938737280852));
#28759=CARTESIAN_POINT('Ctrl Pts',(-1.38420564527715,1.,-1.21938737280852));
#28760=CARTESIAN_POINT('Ctrl Pts',(-1.39361389568796,-1.,-1.22752961899387));
#28761=CARTESIAN_POINT('Ctrl Pts',(-1.39361389568796,1.,-1.22752961899387));
#28762=CARTESIAN_POINT('Ctrl Pts',(-1.40164708206106,-1.,-1.23434087290423));
#28763=CARTESIAN_POINT('Ctrl Pts',(-1.40164708206106,1.,-1.23434087290423));
#28764=CARTESIAN_POINT('Ctrl Pts',(-1.40845295531283,-1.,-1.23994455029534));
#28765=CARTESIAN_POINT('Ctrl Pts',(-1.40845295531283,1.,-1.23994455029534));
#28766=CARTESIAN_POINT('Ctrl Pts',(-1.41422913175179,-1.,-1.24450600513056));
#28767=CARTESIAN_POINT('Ctrl Pts',(-1.41422913175179,1.,-1.24450600513056));
#28768=CARTESIAN_POINT('Ctrl Pts',(-1.41923722596025,-1.,-1.24824430986571));
#28769=CARTESIAN_POINT('Ctrl Pts',(-1.41923722596025,1.,-1.24824430986571));
#28770=CARTESIAN_POINT('Ctrl Pts',(-1.42378102115575,-1.,-1.2514145557001));
#28771=CARTESIAN_POINT('Ctrl Pts',(-1.42378102115575,1.,-1.2514145557001));
#28772=CARTESIAN_POINT('Ctrl Pts',(-1.42815938799387,-1.,-1.25426945222639));
#28773=CARTESIAN_POINT('Ctrl Pts',(-1.42815938799387,1.,-1.25426945222639));
#28774=CARTESIAN_POINT('Ctrl Pts',(-1.43262645609691,-1.,-1.25702687965755));
#28775=CARTESIAN_POINT('Ctrl Pts',(-1.43262645609691,1.,-1.25702687965755));
#28776=CARTESIAN_POINT('Ctrl Pts',(-1.43734919180848,-1.,-1.25983531012005));
#28777=CARTESIAN_POINT('Ctrl Pts',(-1.43734919180848,1.,-1.25983531012005));
#28778=CARTESIAN_POINT('Ctrl Pts',(-1.44236470511303,-1.,-1.26273903323859));
#28779=CARTESIAN_POINT('Ctrl Pts',(-1.44236470511303,1.,-1.26273903323859));
#28780=CARTESIAN_POINT('Ctrl Pts',(-1.44761985001662,-1.,-1.26570925118868));
#28781=CARTESIAN_POINT('Ctrl Pts',(-1.44761985001662,1.,-1.26570925118868));
#28782=CARTESIAN_POINT('Ctrl Pts',(-1.45301422764247,-1.,-1.2686778680489));
#28783=CARTESIAN_POINT('Ctrl Pts',(-1.45301422764247,1.,-1.2686778680489));
#28784=CARTESIAN_POINT('Ctrl Pts',(-1.45843906294697,-1.,-1.27156805265289));
#28785=CARTESIAN_POINT('Ctrl Pts',(-1.45843906294697,1.,-1.27156805265289));
#28786=CARTESIAN_POINT('Ctrl Pts',(-1.46382431332476,-1.,-1.27433119897822));
#28787=CARTESIAN_POINT('Ctrl Pts',(-1.46382431332476,1.,-1.27433119897822));
#28788=CARTESIAN_POINT('Ctrl Pts',(-1.46916035917133,-1.,-1.27696414831089));
#28789=CARTESIAN_POINT('Ctrl Pts',(-1.46916035917133,1.,-1.27696414831089));
#28790=CARTESIAN_POINT('Ctrl Pts',(-1.4744717526707,-1.,-1.2794891824849));
#28791=CARTESIAN_POINT('Ctrl Pts',(-1.4744717526707,1.,-1.2794891824849));
#28792=CARTESIAN_POINT('Ctrl Pts',(-1.47980070347095,-1.,-1.28194158939517));
#28793=CARTESIAN_POINT('Ctrl Pts',(-1.47980070347095,1.,-1.28194158939517));
#28794=CARTESIAN_POINT('Ctrl Pts',(-1.4851881711891,-1.,-1.28435533880201));
#28795=CARTESIAN_POINT('Ctrl Pts',(-1.4851881711891,1.,-1.28435533880201));
#28796=CARTESIAN_POINT('Ctrl Pts',(-1.4906522831278,-1.,-1.2867467611644));
#28797=CARTESIAN_POINT('Ctrl Pts',(-1.4906522831278,1.,-1.2867467611644));
#28798=CARTESIAN_POINT('Ctrl Pts',(-1.49618896881754,-1.,-1.28911506584254));
#28799=CARTESIAN_POINT('Ctrl Pts',(-1.49618896881754,1.,-1.28911506584254));
#28800=CARTESIAN_POINT('Ctrl Pts',(-1.50178230149776,-1.,-1.29145022885181));
#28801=CARTESIAN_POINT('Ctrl Pts',(-1.50178230149776,1.,-1.29145022885181));
#28802=CARTESIAN_POINT('Ctrl Pts',(-1.50741159078365,-1.,-1.29373841372842));
#28803=CARTESIAN_POINT('Ctrl Pts',(-1.50741159078365,1.,-1.29373841372842));
#28804=CARTESIAN_POINT('Ctrl Pts',(-1.51305994241402,-1.,-1.29596850710509));
#28805=CARTESIAN_POINT('Ctrl Pts',(-1.51305994241402,1.,-1.29596850710509));
#28806=CARTESIAN_POINT('Ctrl Pts',(-1.51872184912724,-1.,-1.29813791800747));
#28807=CARTESIAN_POINT('Ctrl Pts',(-1.51872184912724,1.,-1.29813791800747));
#28808=CARTESIAN_POINT('Ctrl Pts',(-1.52439957861062,-1.,-1.30024984366328));
#28809=CARTESIAN_POINT('Ctrl Pts',(-1.52439957861062,1.,-1.30024984366328));
#28810=CARTESIAN_POINT('Ctrl Pts',(-1.53009970283891,-1.,-1.30231064395568));
#28811=CARTESIAN_POINT('Ctrl Pts',(-1.53009970283891,1.,-1.30231064395568));
#28812=CARTESIAN_POINT('Ctrl Pts',(-1.53582981268977,-1.,-1.30432735639489));
#28813=CARTESIAN_POINT('Ctrl Pts',(-1.53582981268977,1.,-1.30432735639489));
#28814=CARTESIAN_POINT('Ctrl Pts',(-1.54159462645432,-1.,-1.30630475189556));
#28815=CARTESIAN_POINT('Ctrl Pts',(-1.54159462645432,1.,-1.30630475189556));
#28816=CARTESIAN_POINT('Ctrl Pts',(-1.54739413957185,-1.,-1.30824393907473));
#28817=CARTESIAN_POINT('Ctrl Pts',(-1.54739413957185,1.,-1.30824393907473));
#28818=CARTESIAN_POINT('Ctrl Pts',(-1.55322568759481,-1.,-1.31014393684222));
#28819=CARTESIAN_POINT('Ctrl Pts',(-1.55322568759481,1.,-1.31014393684222));
#28820=CARTESIAN_POINT('Ctrl Pts',(-1.55908521254821,-1.,-1.31200264341696));
#28821=CARTESIAN_POINT('Ctrl Pts',(-1.55908521254821,1.,-1.31200264341696));
#28822=CARTESIAN_POINT('Ctrl Pts',(-1.56496872402353,-1.,-1.31381795281002));
#28823=CARTESIAN_POINT('Ctrl Pts',(-1.56496872402353,1.,-1.31381795281002));
#28824=CARTESIAN_POINT('Ctrl Pts',(-1.57087397835723,-1.,-1.31558903860016));
#28825=CARTESIAN_POINT('Ctrl Pts',(-1.57087397835723,1.,-1.31558903860016));
#28826=CARTESIAN_POINT('Ctrl Pts',(-1.5768005650559,-1.,-1.31731642317187));
#28827=CARTESIAN_POINT('Ctrl Pts',(-1.5768005650559,1.,-1.31731642317187));
#28828=CARTESIAN_POINT('Ctrl Pts',(-1.58274907898834,-1.,-1.31900135021432));
#28829=CARTESIAN_POINT('Ctrl Pts',(-1.58274907898834,1.,-1.31900135021432));
#28830=CARTESIAN_POINT('Ctrl Pts',(-1.58872057258245,-1.,-1.32064537110892));
#28831=CARTESIAN_POINT('Ctrl Pts',(-1.58872057258245,1.,-1.32064537110892));
#28832=CARTESIAN_POINT('Ctrl Pts',(-1.59471591079403,-1.,-1.32224985747682));
#28833=CARTESIAN_POINT('Ctrl Pts',(-1.59471591079403,1.,-1.32224985747682));
#28834=CARTESIAN_POINT('Ctrl Pts',(-1.60073511858687,-1.,-1.32381550858256));
#28835=CARTESIAN_POINT('Ctrl Pts',(-1.60073511858687,1.,-1.32381550858256));
#28836=CARTESIAN_POINT('Ctrl Pts',(-1.60677758290954,-1.,-1.32534250785782));
#28837=CARTESIAN_POINT('Ctrl Pts',(-1.60677758290954,1.,-1.32534250785782));
#28838=CARTESIAN_POINT('Ctrl Pts',(-1.6128423401575,-1.,-1.32683074483356));
#28839=CARTESIAN_POINT('Ctrl Pts',(-1.6128423401575,1.,-1.32683074483356));
#28840=CARTESIAN_POINT('Ctrl Pts',(-1.61892832270724,-1.,-1.32828000610449));
#28841=CARTESIAN_POINT('Ctrl Pts',(-1.61892832270724,1.,-1.32828000610449));
#28842=CARTESIAN_POINT('Ctrl Pts',(-1.62503464209797,-1.,-1.3296901950568));
#28843=CARTESIAN_POINT('Ctrl Pts',(-1.62503464209797,1.,-1.3296901950568));
#28844=CARTESIAN_POINT('Ctrl Pts',(-1.63116079730923,-1.,-1.33106149345645));
#28845=CARTESIAN_POINT('Ctrl Pts',(-1.63116079730923,1.,-1.33106149345645));
#28846=CARTESIAN_POINT('Ctrl Pts',(-1.63730653475089,-1.,-1.33239425103724));
#28847=CARTESIAN_POINT('Ctrl Pts',(-1.63730653475089,1.,-1.33239425103724));
#28848=CARTESIAN_POINT('Ctrl Pts',(-1.6434717485603,-1.,-1.33368890676572));
#28849=CARTESIAN_POINT('Ctrl Pts',(-1.6434717485603,1.,-1.33368890676572));
#28850=CARTESIAN_POINT('Ctrl Pts',(-1.6496563728683,-1.,-1.33494590467993));
#28851=CARTESIAN_POINT('Ctrl Pts',(-1.6496563728683,1.,-1.33494590467993));
#28852=CARTESIAN_POINT('Ctrl Pts',(-1.65586025952593,-1.,-1.33616559745172));
#28853=CARTESIAN_POINT('Ctrl Pts',(-1.65586025952593,1.,-1.33616559745172));
#28854=CARTESIAN_POINT('Ctrl Pts',(-1.66208312541983,-1.,-1.33734820885262));
#28855=CARTESIAN_POINT('Ctrl Pts',(-1.66208312541983,1.,-1.33734820885262));
#28856=CARTESIAN_POINT('Ctrl Pts',(-1.66832460783989,-1.,-1.33849388654388));
#28857=CARTESIAN_POINT('Ctrl Pts',(-1.66832460783989,1.,-1.33849388654388));
#28858=CARTESIAN_POINT('Ctrl Pts',(-1.67458429426086,-1.,-1.3396027347034));
#28859=CARTESIAN_POINT('Ctrl Pts',(-1.67458429426086,1.,-1.3396027347034));
#28860=CARTESIAN_POINT('Ctrl Pts',(-1.68086176030362,-1.,-1.34067485185203));
#28861=CARTESIAN_POINT('Ctrl Pts',(-1.68086176030362,1.,-1.34067485185203));
#28862=CARTESIAN_POINT('Ctrl Pts',(-1.68715660868764,-1.,-1.341710374848));
#28863=CARTESIAN_POINT('Ctrl Pts',(-1.68715660868764,1.,-1.341710374848));
#28864=CARTESIAN_POINT('Ctrl Pts',(-1.6934684849687,-1.,-1.34270948206319));
#28865=CARTESIAN_POINT('Ctrl Pts',(-1.6934684849687,1.,-1.34270948206319));
#28866=CARTESIAN_POINT('Ctrl Pts',(-1.69979707754427,-1.,-1.34367237124483));
#28867=CARTESIAN_POINT('Ctrl Pts',(-1.69979707754427,1.,-1.34367237124483));
#28868=CARTESIAN_POINT('Ctrl Pts',(-1.70614212266738,-1.,-1.34459924533831));
#28869=CARTESIAN_POINT('Ctrl Pts',(-1.70614212266738,1.,-1.34459924533831));
#28870=CARTESIAN_POINT('Ctrl Pts',(-1.71250340686822,-1.,-1.34549029589416));
#28871=CARTESIAN_POINT('Ctrl Pts',(-1.71250340686822,1.,-1.34549029589416));
#28872=CARTESIAN_POINT('Ctrl Pts',(-1.7188807715049,-1.,-1.34634568653227));
#28873=CARTESIAN_POINT('Ctrl Pts',(-1.7188807715049,1.,-1.34634568653227));
#28874=CARTESIAN_POINT('Ctrl Pts',(-1.72527410680674,-1.,-1.34716554819527));
#28875=CARTESIAN_POINT('Ctrl Pts',(-1.72527410680674,1.,-1.34716554819527));
#28876=CARTESIAN_POINT('Ctrl Pts',(-1.7304014965394,-1.,-1.34779309152035));
#28877=CARTESIAN_POINT('Ctrl Pts',(-1.7304014965394,1.,-1.34779309152035));
#28878=CARTESIAN_POINT('Ctrl Pts',(-1.73425417885907,-1.,-1.34824783112887));
#28879=CARTESIAN_POINT('Ctrl Pts',(-1.73425417885907,1.,-1.34824783112887));
#28880=CARTESIAN_POINT('Ctrl Pts',(-1.73682580585691,-1.,-1.34854391898045));
#28881=CARTESIAN_POINT('Ctrl Pts',(-1.73682580585691,1.,-1.34854391898045));
#28882=CARTESIAN_POINT('Ctrl Pts',(-1.73811241238545,-1.,-1.34869019493419));
#28883=CARTESIAN_POINT('Ctrl Pts',(-1.73811241238545,1.,-1.34869019493419));
#28884=CARTESIAN_POINT('',(-1.31362392696032,1.,-1.15624053661742));
#28885=CARTESIAN_POINT('Ctrl Pts',(-1.31362392696032,1.,-1.15624053661742));
#28886=CARTESIAN_POINT('Ctrl Pts',(-1.31722977216397,1.,-1.15950888730809));
#28887=CARTESIAN_POINT('Ctrl Pts',(-1.32428080721772,1.,-1.16589330093588));
#28888=CARTESIAN_POINT('Ctrl Pts',(-1.33437539347008,1.,-1.17501305789857));
#28889=CARTESIAN_POINT('Ctrl Pts',(-1.34687054001093,1.,-1.18625865667441));
#28890=CARTESIAN_POINT('Ctrl Pts',(-1.36088705043885,1.,-1.1987959077932));
#28891=CARTESIAN_POINT('Ctrl Pts',(-1.37331915607905,1.,-1.20982812925645));
#28892=CARTESIAN_POINT('Ctrl Pts',(-1.38420564527715,1.,-1.21938737280852));
#28893=CARTESIAN_POINT('Ctrl Pts',(-1.39361389568796,1.,-1.22752961899387));
#28894=CARTESIAN_POINT('Ctrl Pts',(-1.40164708206106,1.,-1.23434087290423));
#28895=CARTESIAN_POINT('Ctrl Pts',(-1.40845295531283,1.,-1.23994455029534));
#28896=CARTESIAN_POINT('Ctrl Pts',(-1.41422913175179,1.,-1.24450600513056));
#28897=CARTESIAN_POINT('Ctrl Pts',(-1.41923722596025,1.,-1.24824430986571));
#28898=CARTESIAN_POINT('Ctrl Pts',(-1.42378102115575,1.,-1.2514145557001));
#28899=CARTESIAN_POINT('Ctrl Pts',(-1.42815938799387,1.,-1.25426945222639));
#28900=CARTESIAN_POINT('Ctrl Pts',(-1.43262645609691,1.,-1.25702687965755));
#28901=CARTESIAN_POINT('Ctrl Pts',(-1.43734919180848,1.,-1.25983531012005));
#28902=CARTESIAN_POINT('Ctrl Pts',(-1.44236470511303,1.,-1.26273903323859));
#28903=CARTESIAN_POINT('Ctrl Pts',(-1.44761985001662,1.,-1.26570925118868));
#28904=CARTESIAN_POINT('Ctrl Pts',(-1.45301422764247,1.,-1.2686778680489));
#28905=CARTESIAN_POINT('Ctrl Pts',(-1.45843906294697,1.,-1.27156805265289));
#28906=CARTESIAN_POINT('Ctrl Pts',(-1.46382431332476,1.,-1.27433119897822));
#28907=CARTESIAN_POINT('Ctrl Pts',(-1.46916035917133,1.,-1.27696414831089));
#28908=CARTESIAN_POINT('Ctrl Pts',(-1.4744717526707,1.,-1.2794891824849));
#28909=CARTESIAN_POINT('Ctrl Pts',(-1.47980070347095,1.,-1.28194158939517));
#28910=CARTESIAN_POINT('Ctrl Pts',(-1.4851881711891,1.,-1.28435533880201));
#28911=CARTESIAN_POINT('Ctrl Pts',(-1.4906522831278,1.,-1.2867467611644));
#28912=CARTESIAN_POINT('Ctrl Pts',(-1.49618896881754,1.,-1.28911506584254));
#28913=CARTESIAN_POINT('Ctrl Pts',(-1.50178230149776,1.,-1.29145022885181));
#28914=CARTESIAN_POINT('Ctrl Pts',(-1.50741159078365,1.,-1.29373841372842));
#28915=CARTESIAN_POINT('Ctrl Pts',(-1.51305994241402,1.,-1.29596850710509));
#28916=CARTESIAN_POINT('Ctrl Pts',(-1.51872184912724,1.,-1.29813791800747));
#28917=CARTESIAN_POINT('Ctrl Pts',(-1.52439957861062,1.,-1.30024984366328));
#28918=CARTESIAN_POINT('Ctrl Pts',(-1.53009970283891,1.,-1.30231064395568));
#28919=CARTESIAN_POINT('Ctrl Pts',(-1.53582981268977,1.,-1.30432735639489));
#28920=CARTESIAN_POINT('Ctrl Pts',(-1.54159462645432,1.,-1.30630475189556));
#28921=CARTESIAN_POINT('Ctrl Pts',(-1.54739413957185,1.,-1.30824393907473));
#28922=CARTESIAN_POINT('Ctrl Pts',(-1.55322568759481,1.,-1.31014393684222));
#28923=CARTESIAN_POINT('Ctrl Pts',(-1.55908521254821,1.,-1.31200264341696));
#28924=CARTESIAN_POINT('Ctrl Pts',(-1.56496872402353,1.,-1.31381795281002));
#28925=CARTESIAN_POINT('Ctrl Pts',(-1.57087397835723,1.,-1.31558903860016));
#28926=CARTESIAN_POINT('Ctrl Pts',(-1.5768005650559,1.,-1.31731642317187));
#28927=CARTESIAN_POINT('Ctrl Pts',(-1.58274907898834,1.,-1.31900135021432));
#28928=CARTESIAN_POINT('Ctrl Pts',(-1.58872057258245,1.,-1.32064537110892));
#28929=CARTESIAN_POINT('Ctrl Pts',(-1.59471591079403,1.,-1.32224985747682));
#28930=CARTESIAN_POINT('Ctrl Pts',(-1.60073511858687,1.,-1.32381550858256));
#28931=CARTESIAN_POINT('Ctrl Pts',(-1.60677758290954,1.,-1.32534250785782));
#28932=CARTESIAN_POINT('Ctrl Pts',(-1.6128423401575,1.,-1.32683074483356));
#28933=CARTESIAN_POINT('Ctrl Pts',(-1.61892832270724,1.,-1.32828000610449));
#28934=CARTESIAN_POINT('Ctrl Pts',(-1.62503464209797,1.,-1.3296901950568));
#28935=CARTESIAN_POINT('Ctrl Pts',(-1.63116079730923,1.,-1.33106149345645));
#28936=CARTESIAN_POINT('Ctrl Pts',(-1.63730653475089,1.,-1.33239425103724));
#28937=CARTESIAN_POINT('Ctrl Pts',(-1.6434717485603,1.,-1.33368890676572));
#28938=CARTESIAN_POINT('Ctrl Pts',(-1.6496563728683,1.,-1.33494590467993));
#28939=CARTESIAN_POINT('Ctrl Pts',(-1.65586025952593,1.,-1.33616559745172));
#28940=CARTESIAN_POINT('Ctrl Pts',(-1.66208312541983,1.,-1.33734820885262));
#28941=CARTESIAN_POINT('Ctrl Pts',(-1.66832460783989,1.,-1.33849388654388));
#28942=CARTESIAN_POINT('Ctrl Pts',(-1.67458429426086,1.,-1.3396027347034));
#28943=CARTESIAN_POINT('Ctrl Pts',(-1.68086176030362,1.,-1.34067485185203));
#28944=CARTESIAN_POINT('Ctrl Pts',(-1.68715660868764,1.,-1.341710374848));
#28945=CARTESIAN_POINT('Ctrl Pts',(-1.6934684849687,1.,-1.34270948206319));
#28946=CARTESIAN_POINT('Ctrl Pts',(-1.69979707754427,1.,-1.34367237124483));
#28947=CARTESIAN_POINT('Ctrl Pts',(-1.70614212266738,1.,-1.34459924533831));
#28948=CARTESIAN_POINT('Ctrl Pts',(-1.71250340686822,1.,-1.34549029589416));
#28949=CARTESIAN_POINT('Ctrl Pts',(-1.7188807715049,1.,-1.34634568653227));
#28950=CARTESIAN_POINT('Ctrl Pts',(-1.72527410680674,1.,-1.34716554819527));
#28951=CARTESIAN_POINT('Ctrl Pts',(-1.7304014965394,1.,-1.34779309152035));
#28952=CARTESIAN_POINT('Ctrl Pts',(-1.73425417885907,1.,-1.34824783112887));
#28953=CARTESIAN_POINT('Ctrl Pts',(-1.73682580585691,1.,-1.34854391898045));
#28954=CARTESIAN_POINT('Ctrl Pts',(-1.73811241238545,1.,-1.34869019493419));
#28955=CARTESIAN_POINT('',(-1.31362392696032,0.,-1.15624053661742));
#28956=CARTESIAN_POINT('Origin',(0.,0.,0.));
#28957=CARTESIAN_POINT('',(-1.15624053661742,1.,-1.31362392696033));
#28958=CARTESIAN_POINT('Origin',(0.,1.,0.));
#28959=CARTESIAN_POINT('',(-1.15624053661742,0.,-1.31362392696033));
#28960=CARTESIAN_POINT('Ctrl Pts',(-1.34869019493419,-1.,-1.73811241238545));
#28961=CARTESIAN_POINT('Ctrl Pts',(-1.34869019493419,1.,-1.73811241238545));
#28962=CARTESIAN_POINT('Ctrl Pts',(-1.34854391898145,-1.,-1.73682580585819));
#28963=CARTESIAN_POINT('Ctrl Pts',(-1.34854391898145,1.,-1.73682580585819));
#28964=CARTESIAN_POINT('Ctrl Pts',(-1.34824783113158,-1.,-1.73425417886255));
#28965=CARTESIAN_POINT('Ctrl Pts',(-1.34824783113158,1.,-1.73425417886255));
#28966=CARTESIAN_POINT('Ctrl Pts',(-1.3477930915247,-1.,-1.73040149654497));
#28967=CARTESIAN_POINT('Ctrl Pts',(-1.3477930915247,1.,-1.73040149654497));
#28968=CARTESIAN_POINT('Ctrl Pts',(-1.34716554820013,-1.,-1.72527410681298));
#28969=CARTESIAN_POINT('Ctrl Pts',(-1.34716554820013,1.,-1.72527410681298));
#28970=CARTESIAN_POINT('Ctrl Pts',(-1.34634568653586,-1.,-1.7188807715095));
#28971=CARTESIAN_POINT('Ctrl Pts',(-1.34634568653586,1.,-1.7188807715095));
#28972=CARTESIAN_POINT('Ctrl Pts',(-1.34549029589563,-1.,-1.71250340687011));
#28973=CARTESIAN_POINT('Ctrl Pts',(-1.34549029589563,1.,-1.71250340687011));
#28974=CARTESIAN_POINT('Ctrl Pts',(-1.34459924533783,-1.,-1.70614212266676));
#28975=CARTESIAN_POINT('Ctrl Pts',(-1.34459924533783,1.,-1.70614212266676));
#28976=CARTESIAN_POINT('Ctrl Pts',(-1.34367237124322,-1.,-1.69979707754221));
#28977=CARTESIAN_POINT('Ctrl Pts',(-1.34367237124322,1.,-1.69979707754221));
#28978=CARTESIAN_POINT('Ctrl Pts',(-1.34270948206139,-1.,-1.6934684849664));
#28979=CARTESIAN_POINT('Ctrl Pts',(-1.34270948206139,1.,-1.6934684849664));
#28980=CARTESIAN_POINT('Ctrl Pts',(-1.34171037484673,-1.,-1.68715660868602));
#28981=CARTESIAN_POINT('Ctrl Pts',(-1.34171037484673,1.,-1.68715660868602));
#28982=CARTESIAN_POINT('Ctrl Pts',(-1.3406748518516,-1.,-1.68086176030308));
#28983=CARTESIAN_POINT('Ctrl Pts',(-1.3406748518516,1.,-1.68086176030308));
#28984=CARTESIAN_POINT('Ctrl Pts',(-1.33960273470372,-1.,-1.67458429426126));
#28985=CARTESIAN_POINT('Ctrl Pts',(-1.33960273470372,1.,-1.67458429426126));
#28986=CARTESIAN_POINT('Ctrl Pts',(-1.33849388654458,-1.,-1.66832460784078));
#28987=CARTESIAN_POINT('Ctrl Pts',(-1.33849388654458,1.,-1.66832460784078));
#28988=CARTESIAN_POINT('Ctrl Pts',(-1.33734820885331,-1.,-1.66208312542073));
#28989=CARTESIAN_POINT('Ctrl Pts',(-1.33734820885331,1.,-1.66208312542073));
#28990=CARTESIAN_POINT('Ctrl Pts',(-1.33616559745217,-1.,-1.65586025952651));
#28991=CARTESIAN_POINT('Ctrl Pts',(-1.33616559745217,1.,-1.65586025952651));
#28992=CARTESIAN_POINT('Ctrl Pts',(-1.33494590468003,-1.,-1.64965637286843));
#28993=CARTESIAN_POINT('Ctrl Pts',(-1.33494590468003,1.,-1.64965637286843));
#28994=CARTESIAN_POINT('Ctrl Pts',(-1.33368890676554,-1.,-1.64347174856007));
#28995=CARTESIAN_POINT('Ctrl Pts',(-1.33368890676554,1.,-1.64347174856007));
#28996=CARTESIAN_POINT('Ctrl Pts',(-1.33239425103694,-1.,-1.6373065347505));
#28997=CARTESIAN_POINT('Ctrl Pts',(-1.33239425103694,1.,-1.6373065347505));
#28998=CARTESIAN_POINT('Ctrl Pts',(-1.33106149345618,-1.,-1.63116079730887));
#28999=CARTESIAN_POINT('Ctrl Pts',(-1.33106149345618,1.,-1.63116079730887));
#29000=CARTESIAN_POINT('Ctrl Pts',(-1.32969019505665,-1.,-1.62503464209777));
#29001=CARTESIAN_POINT('Ctrl Pts',(-1.32969019505665,1.,-1.62503464209777));
#29002=CARTESIAN_POINT('Ctrl Pts',(-1.32828000610448,-1.,-1.61892832270723));
#29003=CARTESIAN_POINT('Ctrl Pts',(-1.32828000610448,1.,-1.61892832270723));
#29004=CARTESIAN_POINT('Ctrl Pts',(-1.32683074483365,-1.,-1.61284234015762));
#29005=CARTESIAN_POINT('Ctrl Pts',(-1.32683074483365,1.,-1.61284234015762));
#29006=CARTESIAN_POINT('Ctrl Pts',(-1.32534250785794,-1.,-1.6067775829097));
#29007=CARTESIAN_POINT('Ctrl Pts',(-1.32534250785794,1.,-1.6067775829097));
#29008=CARTESIAN_POINT('Ctrl Pts',(-1.32381550858266,-1.,-1.600735118587));
#29009=CARTESIAN_POINT('Ctrl Pts',(-1.32381550858266,1.,-1.600735118587));
#29010=CARTESIAN_POINT('Ctrl Pts',(-1.32224985747686,-1.,-1.59471591079408));
#29011=CARTESIAN_POINT('Ctrl Pts',(-1.32224985747686,1.,-1.59471591079408));
#29012=CARTESIAN_POINT('Ctrl Pts',(-1.32064537110891,-1.,-1.58872057258244));
#29013=CARTESIAN_POINT('Ctrl Pts',(-1.32064537110891,1.,-1.58872057258244));
#29014=CARTESIAN_POINT('Ctrl Pts',(-1.31900135021428,-1.,-1.58274907898829));
#29015=CARTESIAN_POINT('Ctrl Pts',(-1.31900135021428,1.,-1.58274907898829));
#29016=CARTESIAN_POINT('Ctrl Pts',(-1.31731642317183,-1.,-1.57680056505585));
#29017=CARTESIAN_POINT('Ctrl Pts',(-1.31731642317183,1.,-1.57680056505585));
#29018=CARTESIAN_POINT('Ctrl Pts',(-1.31558903860015,-1.,-1.57087397835721));
#29019=CARTESIAN_POINT('Ctrl Pts',(-1.31558903860015,1.,-1.57087397835721));
#29020=CARTESIAN_POINT('Ctrl Pts',(-1.31381795281002,-1.,-1.56496872402352));
#29021=CARTESIAN_POINT('Ctrl Pts',(-1.31381795281002,1.,-1.56496872402352));
#29022=CARTESIAN_POINT('Ctrl Pts',(-1.31200264341696,-1.,-1.55908521254822));
#29023=CARTESIAN_POINT('Ctrl Pts',(-1.31200264341696,1.,-1.55908521254822));
#29024=CARTESIAN_POINT('Ctrl Pts',(-1.31014393684221,-1.,-1.55322568759481));
#29025=CARTESIAN_POINT('Ctrl Pts',(-1.31014393684221,1.,-1.55322568759481));
#29026=CARTESIAN_POINT('Ctrl Pts',(-1.30824393907471,-1.,-1.54739413957183));
#29027=CARTESIAN_POINT('Ctrl Pts',(-1.30824393907471,1.,-1.54739413957183));
#29028=CARTESIAN_POINT('Ctrl Pts',(-1.30630475189553,-1.,-1.54159462645428));
#29029=CARTESIAN_POINT('Ctrl Pts',(-1.30630475189553,1.,-1.54159462645428));
#29030=CARTESIAN_POINT('Ctrl Pts',(-1.30432735639487,-1.,-1.53582981268976));
#29031=CARTESIAN_POINT('Ctrl Pts',(-1.30432735639487,1.,-1.53582981268976));
#29032=CARTESIAN_POINT('Ctrl Pts',(-1.3023106439557,-1.,-1.53009970283893));
#29033=CARTESIAN_POINT('Ctrl Pts',(-1.3023106439557,1.,-1.53009970283893));
#29034=CARTESIAN_POINT('Ctrl Pts',(-1.30024984366334,-1.,-1.5243995786107));
#29035=CARTESIAN_POINT('Ctrl Pts',(-1.30024984366334,1.,-1.5243995786107));
#29036=CARTESIAN_POINT('Ctrl Pts',(-1.29813791800757,-1.,-1.51872184912735));
#29037=CARTESIAN_POINT('Ctrl Pts',(-1.29813791800757,1.,-1.51872184912735));
#29038=CARTESIAN_POINT('Ctrl Pts',(-1.29596850710518,-1.,-1.51305994241412));
#29039=CARTESIAN_POINT('Ctrl Pts',(-1.29596850710518,1.,-1.51305994241412));
#29040=CARTESIAN_POINT('Ctrl Pts',(-1.29373841372843,-1.,-1.50741159078367));
#29041=CARTESIAN_POINT('Ctrl Pts',(-1.29373841372843,1.,-1.50741159078367));
#29042=CARTESIAN_POINT('Ctrl Pts',(-1.29145022885171,-1.,-1.50178230149764));
#29043=CARTESIAN_POINT('Ctrl Pts',(-1.29145022885171,1.,-1.50178230149764));
#29044=CARTESIAN_POINT('Ctrl Pts',(-1.28911506584232,-1.,-1.49618896881729));
#29045=CARTESIAN_POINT('Ctrl Pts',(-1.28911506584232,1.,-1.49618896881729));
#29046=CARTESIAN_POINT('Ctrl Pts',(-1.28674676116415,-1.,-1.4906522831275));
#29047=CARTESIAN_POINT('Ctrl Pts',(-1.28674676116415,1.,-1.4906522831275));
#29048=CARTESIAN_POINT('Ctrl Pts',(-1.28435533880184,-1.,-1.48518817118891));
#29049=CARTESIAN_POINT('Ctrl Pts',(-1.28435533880184,1.,-1.48518817118891));
#29050=CARTESIAN_POINT('Ctrl Pts',(-1.28194158939522,-1.,-1.47980070347102));
#29051=CARTESIAN_POINT('Ctrl Pts',(-1.28194158939522,1.,-1.47980070347102));
#29052=CARTESIAN_POINT('Ctrl Pts',(-1.27948918248524,-1.,-1.4744717526711));
#29053=CARTESIAN_POINT('Ctrl Pts',(-1.27948918248524,1.,-1.4744717526711));
#29054=CARTESIAN_POINT('Ctrl Pts',(-1.27696414831144,-1.,-1.46916035917197));
#29055=CARTESIAN_POINT('Ctrl Pts',(-1.27696414831144,1.,-1.46916035917197));
#29056=CARTESIAN_POINT('Ctrl Pts',(-1.27433119897877,-1.,-1.4638243133254));
#29057=CARTESIAN_POINT('Ctrl Pts',(-1.27433119897877,1.,-1.4638243133254));
#29058=CARTESIAN_POINT('Ctrl Pts',(-1.27156805265312,-1.,-1.45843906294725));
#29059=CARTESIAN_POINT('Ctrl Pts',(-1.27156805265312,1.,-1.45843906294725));
#29060=CARTESIAN_POINT('Ctrl Pts',(-1.26867786804854,-1.,-1.45301422764205));
#29061=CARTESIAN_POINT('Ctrl Pts',(-1.26867786804854,1.,-1.45301422764205));
#29062=CARTESIAN_POINT('Ctrl Pts',(-1.26570925118767,-1.,-1.44761985001544));
#29063=CARTESIAN_POINT('Ctrl Pts',(-1.26570925118767,1.,-1.44761985001544));
#29064=CARTESIAN_POINT('Ctrl Pts',(-1.26273903323723,-1.,-1.44236470511145));
#29065=CARTESIAN_POINT('Ctrl Pts',(-1.26273903323723,1.,-1.44236470511145));
#29066=CARTESIAN_POINT('Ctrl Pts',(-1.25983531011894,-1.,-1.43734919180719));
#29067=CARTESIAN_POINT('Ctrl Pts',(-1.25983531011894,1.,-1.43734919180719));
#29068=CARTESIAN_POINT('Ctrl Pts',(-1.25702687965744,-1.,-1.43262645609679));
#29069=CARTESIAN_POINT('Ctrl Pts',(-1.25702687965744,1.,-1.43262645609679));
#29070=CARTESIAN_POINT('Ctrl Pts',(-1.25426945222783,-1.,-1.42815938799555));
#29071=CARTESIAN_POINT('Ctrl Pts',(-1.25426945222783,1.,-1.42815938799555));
#29072=CARTESIAN_POINT('Ctrl Pts',(-1.25141455570299,-1.,-1.42378102115911));
#29073=CARTESIAN_POINT('Ctrl Pts',(-1.25141455570299,1.,-1.42378102115911));
#29074=CARTESIAN_POINT('Ctrl Pts',(-1.24824430986911,-1.,-1.41923722596421));
#29075=CARTESIAN_POINT('Ctrl Pts',(-1.24824430986911,1.,-1.41923722596421));
#29076=CARTESIAN_POINT('Ctrl Pts',(-1.24450600513278,-1.,-1.41422913175437));
#29077=CARTESIAN_POINT('Ctrl Pts',(-1.24450600513278,1.,-1.41422913175437));
#29078=CARTESIAN_POINT('Ctrl Pts',(-1.23994455029421,-1.,-1.40845295531151));
#29079=CARTESIAN_POINT('Ctrl Pts',(-1.23994455029421,1.,-1.40845295531151));
#29080=CARTESIAN_POINT('Ctrl Pts',(-1.23434087289768,-1.,-1.40164708205345));
#29081=CARTESIAN_POINT('Ctrl Pts',(-1.23434087289768,1.,-1.40164708205345));
#29082=CARTESIAN_POINT('Ctrl Pts',(-1.22752961898063,-1.,-1.39361389567257));
#29083=CARTESIAN_POINT('Ctrl Pts',(-1.22752961898063,1.,-1.39361389567257));
#29084=CARTESIAN_POINT('Ctrl Pts',(-1.21938737278853,-1.,-1.38420564525391));
#29085=CARTESIAN_POINT('Ctrl Pts',(-1.21938737278853,1.,-1.38420564525391));
#29086=CARTESIAN_POINT('Ctrl Pts',(-1.20982812923113,-1.,-1.37331915604962));
#29087=CARTESIAN_POINT('Ctrl Pts',(-1.20982812923113,1.,-1.37331915604962));
#29088=CARTESIAN_POINT('Ctrl Pts',(-1.1987959077656,-1.,-1.36088705040677));
#29089=CARTESIAN_POINT('Ctrl Pts',(-1.1987959077656,1.,-1.36088705040677));
#29090=CARTESIAN_POINT('Ctrl Pts',(-1.18625865664915,-1.,-1.34687053998157));
#29091=CARTESIAN_POINT('Ctrl Pts',(-1.18625865664915,1.,-1.34687053998157));
#29092=CARTESIAN_POINT('Ctrl Pts',(-1.17501305787994,-1.,-1.33437539344842));
#29093=CARTESIAN_POINT('Ctrl Pts',(-1.17501305787994,1.,-1.33437539344842));
#29094=CARTESIAN_POINT('Ctrl Pts',(-1.16589330092532,-1.,-1.32428080720544));
#29095=CARTESIAN_POINT('Ctrl Pts',(-1.16589330092532,1.,-1.32428080720544));
#29096=CARTESIAN_POINT('Ctrl Pts',(-1.15950888730433,-1.,-1.3172297721596));
#29097=CARTESIAN_POINT('Ctrl Pts',(-1.15950888730433,1.,-1.3172297721596));
#29098=CARTESIAN_POINT('Ctrl Pts',(-1.15624053661742,-1.,-1.31362392696033));
#29099=CARTESIAN_POINT('Ctrl Pts',(-1.15624053661742,1.,-1.31362392696033));
#29100=CARTESIAN_POINT('',(-1.34869019493419,1.,-1.73811241238545));
#29101=CARTESIAN_POINT('Ctrl Pts',(-1.34869019493419,1.,-1.73811241238545));
#29102=CARTESIAN_POINT('Ctrl Pts',(-1.34854391898145,1.,-1.73682580585819));
#29103=CARTESIAN_POINT('Ctrl Pts',(-1.34824783113158,1.,-1.73425417886255));
#29104=CARTESIAN_POINT('Ctrl Pts',(-1.3477930915247,1.,-1.73040149654497));
#29105=CARTESIAN_POINT('Ctrl Pts',(-1.34716554820013,1.,-1.72527410681298));
#29106=CARTESIAN_POINT('Ctrl Pts',(-1.34634568653586,1.,-1.7188807715095));
#29107=CARTESIAN_POINT('Ctrl Pts',(-1.34549029589563,1.,-1.71250340687011));
#29108=CARTESIAN_POINT('Ctrl Pts',(-1.34459924533783,1.,-1.70614212266676));
#29109=CARTESIAN_POINT('Ctrl Pts',(-1.34367237124322,1.,-1.69979707754221));
#29110=CARTESIAN_POINT('Ctrl Pts',(-1.34270948206139,1.,-1.6934684849664));
#29111=CARTESIAN_POINT('Ctrl Pts',(-1.34171037484673,1.,-1.68715660868602));
#29112=CARTESIAN_POINT('Ctrl Pts',(-1.3406748518516,1.,-1.68086176030308));
#29113=CARTESIAN_POINT('Ctrl Pts',(-1.33960273470372,1.,-1.67458429426126));
#29114=CARTESIAN_POINT('Ctrl Pts',(-1.33849388654458,1.,-1.66832460784078));
#29115=CARTESIAN_POINT('Ctrl Pts',(-1.33734820885331,1.,-1.66208312542073));
#29116=CARTESIAN_POINT('Ctrl Pts',(-1.33616559745217,1.,-1.65586025952651));
#29117=CARTESIAN_POINT('Ctrl Pts',(-1.33494590468003,1.,-1.64965637286843));
#29118=CARTESIAN_POINT('Ctrl Pts',(-1.33368890676554,1.,-1.64347174856007));
#29119=CARTESIAN_POINT('Ctrl Pts',(-1.33239425103694,1.,-1.6373065347505));
#29120=CARTESIAN_POINT('Ctrl Pts',(-1.33106149345618,1.,-1.63116079730887));
#29121=CARTESIAN_POINT('Ctrl Pts',(-1.32969019505665,1.,-1.62503464209777));
#29122=CARTESIAN_POINT('Ctrl Pts',(-1.32828000610448,1.,-1.61892832270723));
#29123=CARTESIAN_POINT('Ctrl Pts',(-1.32683074483365,1.,-1.61284234015762));
#29124=CARTESIAN_POINT('Ctrl Pts',(-1.32534250785794,1.,-1.6067775829097));
#29125=CARTESIAN_POINT('Ctrl Pts',(-1.32381550858266,1.,-1.600735118587));
#29126=CARTESIAN_POINT('Ctrl Pts',(-1.32224985747686,1.,-1.59471591079408));
#29127=CARTESIAN_POINT('Ctrl Pts',(-1.32064537110891,1.,-1.58872057258244));
#29128=CARTESIAN_POINT('Ctrl Pts',(-1.31900135021428,1.,-1.58274907898829));
#29129=CARTESIAN_POINT('Ctrl Pts',(-1.31731642317183,1.,-1.57680056505585));
#29130=CARTESIAN_POINT('Ctrl Pts',(-1.31558903860015,1.,-1.57087397835721));
#29131=CARTESIAN_POINT('Ctrl Pts',(-1.31381795281002,1.,-1.56496872402352));
#29132=CARTESIAN_POINT('Ctrl Pts',(-1.31200264341696,1.,-1.55908521254822));
#29133=CARTESIAN_POINT('Ctrl Pts',(-1.31014393684221,1.,-1.55322568759481));
#29134=CARTESIAN_POINT('Ctrl Pts',(-1.30824393907471,1.,-1.54739413957183));
#29135=CARTESIAN_POINT('Ctrl Pts',(-1.30630475189553,1.,-1.54159462645428));
#29136=CARTESIAN_POINT('Ctrl Pts',(-1.30432735639487,1.,-1.53582981268976));
#29137=CARTESIAN_POINT('Ctrl Pts',(-1.3023106439557,1.,-1.53009970283893));
#29138=CARTESIAN_POINT('Ctrl Pts',(-1.30024984366334,1.,-1.5243995786107));
#29139=CARTESIAN_POINT('Ctrl Pts',(-1.29813791800757,1.,-1.51872184912735));
#29140=CARTESIAN_POINT('Ctrl Pts',(-1.29596850710518,1.,-1.51305994241412));
#29141=CARTESIAN_POINT('Ctrl Pts',(-1.29373841372843,1.,-1.50741159078367));
#29142=CARTESIAN_POINT('Ctrl Pts',(-1.29145022885171,1.,-1.50178230149764));
#29143=CARTESIAN_POINT('Ctrl Pts',(-1.28911506584232,1.,-1.49618896881729));
#29144=CARTESIAN_POINT('Ctrl Pts',(-1.28674676116415,1.,-1.4906522831275));
#29145=CARTESIAN_POINT('Ctrl Pts',(-1.28435533880184,1.,-1.48518817118891));
#29146=CARTESIAN_POINT('Ctrl Pts',(-1.28194158939522,1.,-1.47980070347102));
#29147=CARTESIAN_POINT('Ctrl Pts',(-1.27948918248524,1.,-1.4744717526711));
#29148=CARTESIAN_POINT('Ctrl Pts',(-1.27696414831144,1.,-1.46916035917197));
#29149=CARTESIAN_POINT('Ctrl Pts',(-1.27433119897877,1.,-1.4638243133254));
#29150=CARTESIAN_POINT('Ctrl Pts',(-1.27156805265312,1.,-1.45843906294725));
#29151=CARTESIAN_POINT('Ctrl Pts',(-1.26867786804854,1.,-1.45301422764205));
#29152=CARTESIAN_POINT('Ctrl Pts',(-1.26570925118767,1.,-1.44761985001544));
#29153=CARTESIAN_POINT('Ctrl Pts',(-1.26273903323723,1.,-1.44236470511145));
#29154=CARTESIAN_POINT('Ctrl Pts',(-1.25983531011894,1.,-1.43734919180719));
#29155=CARTESIAN_POINT('Ctrl Pts',(-1.25702687965744,1.,-1.43262645609679));
#29156=CARTESIAN_POINT('Ctrl Pts',(-1.25426945222783,1.,-1.42815938799555));
#29157=CARTESIAN_POINT('Ctrl Pts',(-1.25141455570299,1.,-1.42378102115911));
#29158=CARTESIAN_POINT('Ctrl Pts',(-1.24824430986911,1.,-1.41923722596421));
#29159=CARTESIAN_POINT('Ctrl Pts',(-1.24450600513278,1.,-1.41422913175437));
#29160=CARTESIAN_POINT('Ctrl Pts',(-1.23994455029421,1.,-1.40845295531151));
#29161=CARTESIAN_POINT('Ctrl Pts',(-1.23434087289768,1.,-1.40164708205345));
#29162=CARTESIAN_POINT('Ctrl Pts',(-1.22752961898063,1.,-1.39361389567257));
#29163=CARTESIAN_POINT('Ctrl Pts',(-1.21938737278853,1.,-1.38420564525391));
#29164=CARTESIAN_POINT('Ctrl Pts',(-1.20982812923113,1.,-1.37331915604962));
#29165=CARTESIAN_POINT('Ctrl Pts',(-1.1987959077656,1.,-1.36088705040677));
#29166=CARTESIAN_POINT('Ctrl Pts',(-1.18625865664915,1.,-1.34687053998157));
#29167=CARTESIAN_POINT('Ctrl Pts',(-1.17501305787994,1.,-1.33437539344842));
#29168=CARTESIAN_POINT('Ctrl Pts',(-1.16589330092532,1.,-1.32428080720544));
#29169=CARTESIAN_POINT('Ctrl Pts',(-1.15950888730433,1.,-1.3172297721596));
#29170=CARTESIAN_POINT('Ctrl Pts',(-1.15624053661742,1.,-1.31362392696033));
#29171=CARTESIAN_POINT('',(-1.34869019493419,0.,-1.73811241238545));
#29172=CARTESIAN_POINT('Origin',(-1.23627494547115,0.,-1.81978687191668));
#29173=CARTESIAN_POINT('',(-1.23627494547115,1.,-1.81978687191668));
#29174=CARTESIAN_POINT('',(-1.34869019493419,1.,-1.73811241238545));
#29175=CARTESIAN_POINT('',(-1.23627494547115,0.,-1.81978687191668));
#29176=CARTESIAN_POINT('Ctrl Pts',(-0.892032620296855,-1.,-1.5055822144029));
#29177=CARTESIAN_POINT('Ctrl Pts',(-0.892032620296855,1.,-1.5055822144029));
#29178=CARTESIAN_POINT('Ctrl Pts',(-0.894452006967538,-1.,-1.50980486807181));
#29179=CARTESIAN_POINT('Ctrl Pts',(-0.894452006967538,1.,-1.50980486807181));
#29180=CARTESIAN_POINT('Ctrl Pts',(-0.89918504749193,-1.,-1.51805569591479));
#29181=CARTESIAN_POINT('Ctrl Pts',(-0.89918504749193,1.,-1.51805569591479));
#29182=CARTESIAN_POINT('Ctrl Pts',(-0.905967409640499,-1.,-1.52984849890434));
#29183=CARTESIAN_POINT('Ctrl Pts',(-0.905967409640499,1.,-1.52984849890434));
#29184=CARTESIAN_POINT('Ctrl Pts',(-0.91437591904658,-1.,-1.54440491152808));
#29185=CARTESIAN_POINT('Ctrl Pts',(-0.91437591904658,1.,-1.54440491152808));
#29186=CARTESIAN_POINT('Ctrl Pts',(-0.923832188966322,-1.,-1.56065988582509));
#29187=CARTESIAN_POINT('Ctrl Pts',(-0.923832188966322,1.,-1.56065988582509));
#29188=CARTESIAN_POINT('Ctrl Pts',(-0.932246680128849,-1.,-1.57499388385561));
#29189=CARTESIAN_POINT('Ctrl Pts',(-0.932246680128849,1.,-1.57499388385561));
#29190=CARTESIAN_POINT('Ctrl Pts',(-0.939646377909319,-1.,-1.58744937489796));
#29191=CARTESIAN_POINT('Ctrl Pts',(-0.939646377909319,1.,-1.58744937489796));
#29192=CARTESIAN_POINT('Ctrl Pts',(-0.946078063325796,-1.,-1.59810042045408));
#29193=CARTESIAN_POINT('Ctrl Pts',(-0.946078063325796,1.,-1.59810042045408));
#29194=CARTESIAN_POINT('Ctrl Pts',(-0.951613284361248,-1.,-1.60706069897794));
#29195=CARTESIAN_POINT('Ctrl Pts',(-0.951613284361248,1.,-1.60706069897794));
#29196=CARTESIAN_POINT('Ctrl Pts',(-0.956354422921573,-1.,-1.61449324337233));
#29197=CARTESIAN_POINT('Ctrl Pts',(-0.956354422921573,1.,-1.61449324337233));
#29198=CARTESIAN_POINT('Ctrl Pts',(-0.960438326099958,-1.,-1.62061638139929));
#29199=CARTESIAN_POINT('Ctrl Pts',(-0.960438326099958,1.,-1.62061638139929));
#29200=CARTESIAN_POINT('Ctrl Pts',(-0.964046107037821,-1.,-1.6257193066974));
#29201=CARTESIAN_POINT('Ctrl Pts',(-0.964046107037821,1.,-1.6257193066974));
#29202=CARTESIAN_POINT('Ctrl Pts',(-0.967387853228041,-1.,-1.63013849959083));
#29203=CARTESIAN_POINT('Ctrl Pts',(-0.967387853228041,1.,-1.63013849959083));
#29204=CARTESIAN_POINT('Ctrl Pts',(-0.970669715996356,-1.,-1.63420665729609));
#29205=CARTESIAN_POINT('Ctrl Pts',(-0.970669715996356,1.,-1.63420665729609));
#29206=CARTESIAN_POINT('Ctrl Pts',(-0.974066058287501,-1.,-1.63820952658157));
#29207=CARTESIAN_POINT('Ctrl Pts',(-0.974066058287501,1.,-1.63820952658157));
#29208=CARTESIAN_POINT('Ctrl Pts',(-0.977689794120297,-1.,-1.64233990826831));
#29209=CARTESIAN_POINT('Ctrl Pts',(-0.977689794120297,1.,-1.64233990826831));
#29210=CARTESIAN_POINT('Ctrl Pts',(-0.981562530940574,-1.,-1.64665139190834));
#29211=CARTESIAN_POINT('Ctrl Pts',(-0.981562530940574,1.,-1.64665139190834));
#29212=CARTESIAN_POINT('Ctrl Pts',(-0.985642622921626,-1.,-1.6511001661277));
#29213=CARTESIAN_POINT('Ctrl Pts',(-0.985642622921626,1.,-1.6511001661277));
#29214=CARTESIAN_POINT('Ctrl Pts',(-0.98985562785445,-1.,-1.65559044289746));
#29215=CARTESIAN_POINT('Ctrl Pts',(-0.98985562785445,1.,-1.65559044289746));
#29216=CARTESIAN_POINT('Ctrl Pts',(-0.994121836661116,-1.,-1.66001553809916));
#29217=CARTESIAN_POINT('Ctrl Pts',(-0.994121836661116,1.,-1.66001553809916));
#29218=CARTESIAN_POINT('Ctrl Pts',(-0.998389654952317,-1.,-1.66430758030304));
#29219=CARTESIAN_POINT('Ctrl Pts',(-0.998389654952317,1.,-1.66430758030304));
#29220=CARTESIAN_POINT('Ctrl Pts',(-1.00265091003682,-1.,-1.66846059277231));
#29221=CARTESIAN_POINT('Ctrl Pts',(-1.00265091003682,1.,-1.66846059277231));
#29222=CARTESIAN_POINT('Ctrl Pts',(-1.00692206696387,-1.,-1.67250335383248));
#29223=CARTESIAN_POINT('Ctrl Pts',(-1.00692206696387,1.,-1.67250335383248));
#29224=CARTESIAN_POINT('Ctrl Pts',(-1.01123236493507,-1.,-1.67648246776457));
#29225=CARTESIAN_POINT('Ctrl Pts',(-1.01123236493507,1.,-1.67648246776457));
#29226=CARTESIAN_POINT('Ctrl Pts',(-1.01561026162787,-1.,-1.6804428989482));
#29227=CARTESIAN_POINT('Ctrl Pts',(-1.01561026162787,1.,-1.6804428989482));
#29228=CARTESIAN_POINT('Ctrl Pts',(-1.02006795074222,-1.,-1.68440578021739));
#29229=CARTESIAN_POINT('Ctrl Pts',(-1.02006795074222,1.,-1.68440578021739));
#29230=CARTESIAN_POINT('Ctrl Pts',(-1.02460180535272,-1.,-1.68836910178475));
#29231=CARTESIAN_POINT('Ctrl Pts',(-1.02460180535272,1.,-1.68836910178475));
#29232=CARTESIAN_POINT('Ctrl Pts',(-1.02919977579155,-1.,-1.69231840863471));
#29233=CARTESIAN_POINT('Ctrl Pts',(-1.02919977579155,1.,-1.69231840863471));
#29234=CARTESIAN_POINT('Ctrl Pts',(-1.03384646003587,-1.,-1.69623414782769));
#29235=CARTESIAN_POINT('Ctrl Pts',(-1.03384646003587,1.,-1.69623414782769));
#29236=CARTESIAN_POINT('Ctrl Pts',(-1.03852922490782,-1.,-1.70010052930951));
#29237=CARTESIAN_POINT('Ctrl Pts',(-1.03852922490782,1.,-1.70010052930951));
#29238=CARTESIAN_POINT('Ctrl Pts',(-1.04324363334546,-1.,-1.70391338707969));
#29239=CARTESIAN_POINT('Ctrl Pts',(-1.04324363334546,1.,-1.70391338707969));
#29240=CARTESIAN_POINT('Ctrl Pts',(-1.0479908540499,-1.,-1.70767646263641));
#29241=CARTESIAN_POINT('Ctrl Pts',(-1.0479908540499,1.,-1.70767646263641));
#29242=CARTESIAN_POINT('Ctrl Pts',(-1.05277517202854,-1.,-1.71139783543986));
#29243=CARTESIAN_POINT('Ctrl Pts',(-1.05277517202854,1.,-1.71139783543986));
#29244=CARTESIAN_POINT('Ctrl Pts',(-1.05760163192481,-1.,-1.71508654427022));
#29245=CARTESIAN_POINT('Ctrl Pts',(-1.05760163192481,1.,-1.71508654427022));
#29246=CARTESIAN_POINT('Ctrl Pts',(-1.0624732468065,-1.,-1.71874858456908));
#29247=CARTESIAN_POINT('Ctrl Pts',(-1.0624732468065,1.,-1.71874858456908));
#29248=CARTESIAN_POINT('Ctrl Pts',(-1.06738966975463,-1.,-1.72238500928456));
#29249=CARTESIAN_POINT('Ctrl Pts',(-1.06738966975463,1.,-1.72238500928456));
#29250=CARTESIAN_POINT('Ctrl Pts',(-1.07234866990252,-1.,-1.72599406198489));
#29251=CARTESIAN_POINT('Ctrl Pts',(-1.07234866990252,1.,-1.72599406198489));
#29252=CARTESIAN_POINT('Ctrl Pts',(-1.0773470373727,-1.,-1.72957248977424));
#29253=CARTESIAN_POINT('Ctrl Pts',(-1.0773470373727,1.,-1.72957248977424));
#29254=CARTESIAN_POINT('Ctrl Pts',(-1.08238162784749,-1.,-1.73311705663407));
#29255=CARTESIAN_POINT('Ctrl Pts',(-1.08238162784749,1.,-1.73311705663407));
#29256=CARTESIAN_POINT('Ctrl Pts',(-1.08745056285429,-1.,-1.73662628326093));
#29257=CARTESIAN_POINT('Ctrl Pts',(-1.08745056285429,1.,-1.73662628326093));
#29258=CARTESIAN_POINT('Ctrl Pts',(-1.09255329056496,-1.,-1.74010053962252));
#29259=CARTESIAN_POINT('Ctrl Pts',(-1.09255329056496,1.,-1.74010053962252));
#29260=CARTESIAN_POINT('Ctrl Pts',(-1.09768999241229,-1.,-1.74354119236212));
#29261=CARTESIAN_POINT('Ctrl Pts',(-1.09768999241229,1.,-1.74354119236212));
#29262=CARTESIAN_POINT('Ctrl Pts',(-1.10286118991144,-1.,-1.74695004214924));
#29263=CARTESIAN_POINT('Ctrl Pts',(-1.10286118991144,1.,-1.74695004214924));
#29264=CARTESIAN_POINT('Ctrl Pts',(-1.10806728183003,-1.,-1.75032866075914));
#29265=CARTESIAN_POINT('Ctrl Pts',(-1.10806728183003,1.,-1.75032866075914));
#29266=CARTESIAN_POINT('Ctrl Pts',(-1.11330807582542,-1.,-1.75367772094617));
#29267=CARTESIAN_POINT('Ctrl Pts',(-1.11330807582542,1.,-1.75367772094617));
#29268=CARTESIAN_POINT('Ctrl Pts',(-1.11858293216752,-1.,-1.75699720772089));
#29269=CARTESIAN_POINT('Ctrl Pts',(-1.11858293216752,1.,-1.75699720772089));
#29270=CARTESIAN_POINT('Ctrl Pts',(-1.12389096855078,-1.,-1.76028671825084));
#29271=CARTESIAN_POINT('Ctrl Pts',(-1.12389096855078,1.,-1.76028671825084));
#29272=CARTESIAN_POINT('Ctrl Pts',(-1.12923123555076,-1.,-1.76354571966171));
#29273=CARTESIAN_POINT('Ctrl Pts',(-1.12923123555076,1.,-1.76354571966171));
#29274=CARTESIAN_POINT('Ctrl Pts',(-1.13460291804635,-1.,-1.76677384551883));
#29275=CARTESIAN_POINT('Ctrl Pts',(-1.13460291804635,1.,-1.76677384551883));
#29276=CARTESIAN_POINT('Ctrl Pts',(-1.14000548337,-1.,-1.76997111386806));
#29277=CARTESIAN_POINT('Ctrl Pts',(-1.14000548337,1.,-1.76997111386806));
#29278=CARTESIAN_POINT('Ctrl Pts',(-1.14543858226948,-1.,-1.77313777896234));
#29279=CARTESIAN_POINT('Ctrl Pts',(-1.14543858226948,1.,-1.77313777896234));
#29280=CARTESIAN_POINT('Ctrl Pts',(-1.15090197841531,-1.,-1.77627422557034));
#29281=CARTESIAN_POINT('Ctrl Pts',(-1.15090197841531,1.,-1.77627422557034));
#29282=CARTESIAN_POINT('Ctrl Pts',(-1.15639547194689,-1.,-1.77938085564261));
#29283=CARTESIAN_POINT('Ctrl Pts',(-1.15639547194689,1.,-1.77938085564261));
#29284=CARTESIAN_POINT('Ctrl Pts',(-1.16191881298458,-1.,-1.78245795880949));
#29285=CARTESIAN_POINT('Ctrl Pts',(-1.16191881298458,1.,-1.78245795880949));
#29286=CARTESIAN_POINT('Ctrl Pts',(-1.16747166312239,-1.,-1.78550566040349));
#29287=CARTESIAN_POINT('Ctrl Pts',(-1.16747166312239,1.,-1.78550566040349));
#29288=CARTESIAN_POINT('Ctrl Pts',(-1.17305363177265,-1.,-1.78852398877523));
#29289=CARTESIAN_POINT('Ctrl Pts',(-1.17305363177265,1.,-1.78852398877523));
#29290=CARTESIAN_POINT('Ctrl Pts',(-1.17866429440781,-1.,-1.79151291552646));
#29291=CARTESIAN_POINT('Ctrl Pts',(-1.17866429440781,1.,-1.79151291552646));
#29292=CARTESIAN_POINT('Ctrl Pts',(-1.18430321697471,-1.,-1.79447240321572));
#29293=CARTESIAN_POINT('Ctrl Pts',(-1.18430321697471,1.,-1.79447240321572));
#29294=CARTESIAN_POINT('Ctrl Pts',(-1.1899699793456,-1.,-1.79740245923649));
#29295=CARTESIAN_POINT('Ctrl Pts',(-1.1899699793456,1.,-1.79740245923649));
#29296=CARTESIAN_POINT('Ctrl Pts',(-1.19566418930405,-1.,-1.80030314370121));
#29297=CARTESIAN_POINT('Ctrl Pts',(-1.19566418930405,1.,-1.80030314370121));
#29298=CARTESIAN_POINT('Ctrl Pts',(-1.2013854893912,-1.,-1.8031745483882));
#29299=CARTESIAN_POINT('Ctrl Pts',(-1.2013854893912,1.,-1.8031745483882));
#29300=CARTESIAN_POINT('Ctrl Pts',(-1.20713356605519,-1.,-1.80601678480772));
#29301=CARTESIAN_POINT('Ctrl Pts',(-1.20713356605519,1.,-1.80601678480772));
#29302=CARTESIAN_POINT('Ctrl Pts',(-1.2129081570818,-1.,-1.80882996916931));
#29303=CARTESIAN_POINT('Ctrl Pts',(-1.2129081570818,1.,-1.80882996916931));
#29304=CARTESIAN_POINT('Ctrl Pts',(-1.2187090610323,-1.,-1.81161420806172));
#29305=CARTESIAN_POINT('Ctrl Pts',(-1.2187090610323,1.,-1.81161420806172));
#29306=CARTESIAN_POINT('Ctrl Pts',(-1.22453613304507,-1.,-1.81436959209778));
#29307=CARTESIAN_POINT('Ctrl Pts',(-1.22453613304507,1.,-1.81436959209778));
#29308=CARTESIAN_POINT('Ctrl Pts',(-1.22921864890975,-1.,-1.81655087183054));
#29309=CARTESIAN_POINT('Ctrl Pts',(-1.22921864890975,1.,-1.81655087183054));
#29310=CARTESIAN_POINT('Ctrl Pts',(-1.23274224526804,-1.,-1.81817389920914));
#29311=CARTESIAN_POINT('Ctrl Pts',(-1.23274224526804,1.,-1.81817389920914));
#29312=CARTESIAN_POINT('Ctrl Pts',(-1.23509651170384,-1.,-1.81925017193531));
#29313=CARTESIAN_POINT('Ctrl Pts',(-1.23509651170384,1.,-1.81925017193531));
#29314=CARTESIAN_POINT('Ctrl Pts',(-1.23627494547115,-1.,-1.81978687191668));
#29315=CARTESIAN_POINT('Ctrl Pts',(-1.23627494547115,1.,-1.81978687191668));
#29316=CARTESIAN_POINT('',(-0.892032620296855,1.,-1.5055822144029));
#29317=CARTESIAN_POINT('Ctrl Pts',(-0.892032620296855,1.,-1.5055822144029));
#29318=CARTESIAN_POINT('Ctrl Pts',(-0.894452006967538,1.,-1.50980486807181));
#29319=CARTESIAN_POINT('Ctrl Pts',(-0.89918504749193,1.,-1.51805569591479));
#29320=CARTESIAN_POINT('Ctrl Pts',(-0.905967409640499,1.,-1.52984849890434));
#29321=CARTESIAN_POINT('Ctrl Pts',(-0.91437591904658,1.,-1.54440491152808));
#29322=CARTESIAN_POINT('Ctrl Pts',(-0.923832188966322,1.,-1.56065988582509));
#29323=CARTESIAN_POINT('Ctrl Pts',(-0.932246680128849,1.,-1.57499388385561));
#29324=CARTESIAN_POINT('Ctrl Pts',(-0.939646377909319,1.,-1.58744937489796));
#29325=CARTESIAN_POINT('Ctrl Pts',(-0.946078063325796,1.,-1.59810042045408));
#29326=CARTESIAN_POINT('Ctrl Pts',(-0.951613284361248,1.,-1.60706069897794));
#29327=CARTESIAN_POINT('Ctrl Pts',(-0.956354422921573,1.,-1.61449324337233));
#29328=CARTESIAN_POINT('Ctrl Pts',(-0.960438326099958,1.,-1.62061638139929));
#29329=CARTESIAN_POINT('Ctrl Pts',(-0.964046107037821,1.,-1.6257193066974));
#29330=CARTESIAN_POINT('Ctrl Pts',(-0.967387853228041,1.,-1.63013849959083));
#29331=CARTESIAN_POINT('Ctrl Pts',(-0.970669715996356,1.,-1.63420665729609));
#29332=CARTESIAN_POINT('Ctrl Pts',(-0.974066058287501,1.,-1.63820952658157));
#29333=CARTESIAN_POINT('Ctrl Pts',(-0.977689794120297,1.,-1.64233990826831));
#29334=CARTESIAN_POINT('Ctrl Pts',(-0.981562530940574,1.,-1.64665139190834));
#29335=CARTESIAN_POINT('Ctrl Pts',(-0.985642622921626,1.,-1.6511001661277));
#29336=CARTESIAN_POINT('Ctrl Pts',(-0.98985562785445,1.,-1.65559044289746));
#29337=CARTESIAN_POINT('Ctrl Pts',(-0.994121836661116,1.,-1.66001553809916));
#29338=CARTESIAN_POINT('Ctrl Pts',(-0.998389654952317,1.,-1.66430758030304));
#29339=CARTESIAN_POINT('Ctrl Pts',(-1.00265091003682,1.,-1.66846059277231));
#29340=CARTESIAN_POINT('Ctrl Pts',(-1.00692206696387,1.,-1.67250335383248));
#29341=CARTESIAN_POINT('Ctrl Pts',(-1.01123236493507,1.,-1.67648246776457));
#29342=CARTESIAN_POINT('Ctrl Pts',(-1.01561026162787,1.,-1.6804428989482));
#29343=CARTESIAN_POINT('Ctrl Pts',(-1.02006795074222,1.,-1.68440578021739));
#29344=CARTESIAN_POINT('Ctrl Pts',(-1.02460180535272,1.,-1.68836910178475));
#29345=CARTESIAN_POINT('Ctrl Pts',(-1.02919977579155,1.,-1.69231840863471));
#29346=CARTESIAN_POINT('Ctrl Pts',(-1.03384646003587,1.,-1.69623414782769));
#29347=CARTESIAN_POINT('Ctrl Pts',(-1.03852922490782,1.,-1.70010052930951));
#29348=CARTESIAN_POINT('Ctrl Pts',(-1.04324363334546,1.,-1.70391338707969));
#29349=CARTESIAN_POINT('Ctrl Pts',(-1.0479908540499,1.,-1.70767646263641));
#29350=CARTESIAN_POINT('Ctrl Pts',(-1.05277517202854,1.,-1.71139783543986));
#29351=CARTESIAN_POINT('Ctrl Pts',(-1.05760163192481,1.,-1.71508654427022));
#29352=CARTESIAN_POINT('Ctrl Pts',(-1.0624732468065,1.,-1.71874858456908));
#29353=CARTESIAN_POINT('Ctrl Pts',(-1.06738966975463,1.,-1.72238500928456));
#29354=CARTESIAN_POINT('Ctrl Pts',(-1.07234866990252,1.,-1.72599406198489));
#29355=CARTESIAN_POINT('Ctrl Pts',(-1.0773470373727,1.,-1.72957248977424));
#29356=CARTESIAN_POINT('Ctrl Pts',(-1.08238162784749,1.,-1.73311705663407));
#29357=CARTESIAN_POINT('Ctrl Pts',(-1.08745056285429,1.,-1.73662628326093));
#29358=CARTESIAN_POINT('Ctrl Pts',(-1.09255329056496,1.,-1.74010053962252));
#29359=CARTESIAN_POINT('Ctrl Pts',(-1.09768999241229,1.,-1.74354119236212));
#29360=CARTESIAN_POINT('Ctrl Pts',(-1.10286118991144,1.,-1.74695004214924));
#29361=CARTESIAN_POINT('Ctrl Pts',(-1.10806728183003,1.,-1.75032866075914));
#29362=CARTESIAN_POINT('Ctrl Pts',(-1.11330807582542,1.,-1.75367772094617));
#29363=CARTESIAN_POINT('Ctrl Pts',(-1.11858293216752,1.,-1.75699720772089));
#29364=CARTESIAN_POINT('Ctrl Pts',(-1.12389096855078,1.,-1.76028671825084));
#29365=CARTESIAN_POINT('Ctrl Pts',(-1.12923123555076,1.,-1.76354571966171));
#29366=CARTESIAN_POINT('Ctrl Pts',(-1.13460291804635,1.,-1.76677384551883));
#29367=CARTESIAN_POINT('Ctrl Pts',(-1.14000548337,1.,-1.76997111386806));
#29368=CARTESIAN_POINT('Ctrl Pts',(-1.14543858226948,1.,-1.77313777896234));
#29369=CARTESIAN_POINT('Ctrl Pts',(-1.15090197841531,1.,-1.77627422557034));
#29370=CARTESIAN_POINT('Ctrl Pts',(-1.15639547194689,1.,-1.77938085564261));
#29371=CARTESIAN_POINT('Ctrl Pts',(-1.16191881298458,1.,-1.78245795880949));
#29372=CARTESIAN_POINT('Ctrl Pts',(-1.16747166312239,1.,-1.78550566040349));
#29373=CARTESIAN_POINT('Ctrl Pts',(-1.17305363177265,1.,-1.78852398877523));
#29374=CARTESIAN_POINT('Ctrl Pts',(-1.17866429440781,1.,-1.79151291552646));
#29375=CARTESIAN_POINT('Ctrl Pts',(-1.18430321697471,1.,-1.79447240321572));
#29376=CARTESIAN_POINT('Ctrl Pts',(-1.1899699793456,1.,-1.79740245923649));
#29377=CARTESIAN_POINT('Ctrl Pts',(-1.19566418930405,1.,-1.80030314370121));
#29378=CARTESIAN_POINT('Ctrl Pts',(-1.2013854893912,1.,-1.8031745483882));
#29379=CARTESIAN_POINT('Ctrl Pts',(-1.20713356605519,1.,-1.80601678480772));
#29380=CARTESIAN_POINT('Ctrl Pts',(-1.2129081570818,1.,-1.80882996916931));
#29381=CARTESIAN_POINT('Ctrl Pts',(-1.2187090610323,1.,-1.81161420806172));
#29382=CARTESIAN_POINT('Ctrl Pts',(-1.22453613304507,1.,-1.81436959209778));
#29383=CARTESIAN_POINT('Ctrl Pts',(-1.22921864890975,1.,-1.81655087183054));
#29384=CARTESIAN_POINT('Ctrl Pts',(-1.23274224526804,1.,-1.81817389920914));
#29385=CARTESIAN_POINT('Ctrl Pts',(-1.23509651170384,1.,-1.81925017193531));
#29386=CARTESIAN_POINT('Ctrl Pts',(-1.23627494547115,1.,-1.81978687191668));
#29387=CARTESIAN_POINT('',(-0.892032620296856,0.,-1.5055822144029));
#29388=CARTESIAN_POINT('Origin',(0.,0.,0.));
#29389=CARTESIAN_POINT('',(-0.693717979106305,1.,-1.60662857109684));
#29390=CARTESIAN_POINT('Origin',(0.,1.,0.));
#29391=CARTESIAN_POINT('',(-0.693717979106306,0.,-1.60662857109684));
#29392=CARTESIAN_POINT('Ctrl Pts',(-0.745574324794401,-1.,-2.0698113262342));
#29393=CARTESIAN_POINT('Ctrl Pts',(-0.745574324794401,1.,-2.0698113262342));
#29394=CARTESIAN_POINT('Ctrl Pts',(-0.745832791378367,-1.,-2.06854248895728));
#29395=CARTESIAN_POINT('Ctrl Pts',(-0.745832791378367,1.,-2.06854248895728));
#29396=CARTESIAN_POINT('Ctrl Pts',(-0.7463458715442,-1.,-2.06600523016815));
#29397=CARTESIAN_POINT('Ctrl Pts',(-0.7463458715442,1.,-2.06600523016815));
#29398=CARTESIAN_POINT('Ctrl Pts',(-0.747103932787919,-1.,-2.06220058927826));
#29399=CARTESIAN_POINT('Ctrl Pts',(-0.747103932787919,1.,-2.06220058927826));
#29400=CARTESIAN_POINT('Ctrl Pts',(-0.748091554183802,-1.,-2.05713023031006));
#29401=CARTESIAN_POINT('Ctrl Pts',(-0.748091554183802,1.,-2.05713023031006));
#29402=CARTESIAN_POINT('Ctrl Pts',(-0.749287468665046,-1.,-2.05079645592154));
#29403=CARTESIAN_POINT('Ctrl Pts',(-0.749287468665046,1.,-2.05079645592154));
#29404=CARTESIAN_POINT('Ctrl Pts',(-0.750444657875576,-1.,-2.04446689147979));
#29405=CARTESIAN_POINT('Ctrl Pts',(-0.750444657875576,1.,-2.04446689147979));
#29406=CARTESIAN_POINT('Ctrl Pts',(-0.751562963361115,-1.,-2.03814160092099));
#29407=CARTESIAN_POINT('Ctrl Pts',(-0.751562963361115,1.,-2.03814160092099));
#29408=CARTESIAN_POINT('Ctrl Pts',(-0.752642180487211,-1.,-2.03182068456221));
#29409=CARTESIAN_POINT('Ctrl Pts',(-0.752642180487211,1.,-2.03182068456221));
#29410=CARTESIAN_POINT('Ctrl Pts',(-0.753682061112768,-1.,-2.02550428623313));
#29411=CARTESIAN_POINT('Ctrl Pts',(-0.753682061112768,1.,-2.02550428623313));
#29412=CARTESIAN_POINT('Ctrl Pts',(-0.754682330722816,-1.,-2.01919259405809));
#29413=CARTESIAN_POINT('Ctrl Pts',(-0.754682330722816,1.,-2.01919259405809));
#29414=CARTESIAN_POINT('Ctrl Pts',(-0.755642704957865,-1.,-2.01288584328084));
#29415=CARTESIAN_POINT('Ctrl Pts',(-0.755642704957865,1.,-2.01288584328084));
#29416=CARTESIAN_POINT('Ctrl Pts',(-0.75656290464667,-1.,-2.0065843158773));
#29417=CARTESIAN_POINT('Ctrl Pts',(-0.75656290464667,1.,-2.0065843158773));
#29418=CARTESIAN_POINT('Ctrl Pts',(-0.757442676862724,-1.,-2.00028834739178));
#29419=CARTESIAN_POINT('Ctrl Pts',(-0.757442676862724,1.,-2.00028834739178));
#29420=CARTESIAN_POINT('Ctrl Pts',(-0.758281796766761,-1.,-1.99399831098817));
#29421=CARTESIAN_POINT('Ctrl Pts',(-0.758281796766761,1.,-1.99399831098817));
#29422=CARTESIAN_POINT('Ctrl Pts',(-0.759080037802488,-1.,-1.98771456680874));
#29423=CARTESIAN_POINT('Ctrl Pts',(-0.759080037802488,1.,-1.98771456680874));
#29424=CARTESIAN_POINT('Ctrl Pts',(-0.75983714745219,-1.,-1.98143741418172));
#29425=CARTESIAN_POINT('Ctrl Pts',(-0.75983714745219,1.,-1.98143741418172));
#29426=CARTESIAN_POINT('Ctrl Pts',(-0.760552825409757,-1.,-1.97516705321494));
#29427=CARTESIAN_POINT('Ctrl Pts',(-0.760552825409757,1.,-1.97516705321494));
#29428=CARTESIAN_POINT('Ctrl Pts',(-0.76122669048382,-1.,-1.96890351582499));
#29429=CARTESIAN_POINT('Ctrl Pts',(-0.76122669048382,1.,-1.96890351582499));
#29430=CARTESIAN_POINT('Ctrl Pts',(-0.761858300014423,-1.,-1.96264672744186));
#29431=CARTESIAN_POINT('Ctrl Pts',(-0.761858300014423,1.,-1.96264672744186));
#29432=CARTESIAN_POINT('Ctrl Pts',(-0.762447203806179,-1.,-1.95639665309869));
#29433=CARTESIAN_POINT('Ctrl Pts',(-0.762447203806179,1.,-1.95639665309869));
#29434=CARTESIAN_POINT('Ctrl Pts',(-0.762992990878769,-1.,-1.95015342590024));
#29435=CARTESIAN_POINT('Ctrl Pts',(-0.762992990878769,1.,-1.95015342590024));
#29436=CARTESIAN_POINT('Ctrl Pts',(-0.763495333538629,-1.,-1.9439174661764));
#29437=CARTESIAN_POINT('Ctrl Pts',(-0.763495333538629,1.,-1.9439174661764));
#29438=CARTESIAN_POINT('Ctrl Pts',(-0.763954049121458,-1.,-1.93768964875886));
#29439=CARTESIAN_POINT('Ctrl Pts',(-0.763954049121458,1.,-1.93768964875886));
#29440=CARTESIAN_POINT('Ctrl Pts',(-0.764369010673941,-1.,-1.93147105496382));
#29441=CARTESIAN_POINT('Ctrl Pts',(-0.764369010673941,1.,-1.93147105496382));
#29442=CARTESIAN_POINT('Ctrl Pts',(-0.764740025488211,-1.,-1.92526263537048));
#29443=CARTESIAN_POINT('Ctrl Pts',(-0.764740025488211,1.,-1.92526263537048));
#29444=CARTESIAN_POINT('Ctrl Pts',(-0.765066729667088,-1.,-1.91906491634196));
#29445=CARTESIAN_POINT('Ctrl Pts',(-0.765066729667088,1.,-1.91906491634196));
#29446=CARTESIAN_POINT('Ctrl Pts',(-0.765348465884722,-1.,-1.91287765805169));
#29447=CARTESIAN_POINT('Ctrl Pts',(-0.765348465884722,1.,-1.91287765805169));
#29448=CARTESIAN_POINT('Ctrl Pts',(-0.765584196937919,-1.,-1.90669961402356));
#29449=CARTESIAN_POINT('Ctrl Pts',(-0.765584196937919,1.,-1.90669961402356));
#29450=CARTESIAN_POINT('Ctrl Pts',(-0.765772772593386,-1.,-1.90052930393596));
#29451=CARTESIAN_POINT('Ctrl Pts',(-0.765772772593386,1.,-1.90052930393596));
#29452=CARTESIAN_POINT('Ctrl Pts',(-0.765913193856978,-1.,-1.89436577771388));
#29453=CARTESIAN_POINT('Ctrl Pts',(-0.765913193856978,1.,-1.89436577771388));
#29454=CARTESIAN_POINT('Ctrl Pts',(-0.766004837062091,-1.,-1.88820926433409));
#29455=CARTESIAN_POINT('Ctrl Pts',(-0.766004837062091,1.,-1.88820926433409));
#29456=CARTESIAN_POINT('Ctrl Pts',(-0.766047794851865,-1.,-1.88206215302561));
#29457=CARTESIAN_POINT('Ctrl Pts',(-0.766047794851865,1.,-1.88206215302561));
#29458=CARTESIAN_POINT('Ctrl Pts',(-0.766042837036744,-1.,-1.87592888967883));
#29459=CARTESIAN_POINT('Ctrl Pts',(-0.766042837036744,1.,-1.87592888967883));
#29460=CARTESIAN_POINT('Ctrl Pts',(-0.765990708546091,-1.,-1.86981398314341));
#29461=CARTESIAN_POINT('Ctrl Pts',(-0.765990708546091,1.,-1.86981398314341));
#29462=CARTESIAN_POINT('Ctrl Pts',(-0.765891519092547,-1.,-1.86372027063312));
#29463=CARTESIAN_POINT('Ctrl Pts',(-0.765891519092547,1.,-1.86372027063312));
#29464=CARTESIAN_POINT('Ctrl Pts',(-0.765744212909318,-1.,-1.85764741390394));
#29465=CARTESIAN_POINT('Ctrl Pts',(-0.765744212909318,1.,-1.85764741390394));
#29466=CARTESIAN_POINT('Ctrl Pts',(-0.765545710619062,-1.,-1.85158945130063));
#29467=CARTESIAN_POINT('Ctrl Pts',(-0.765545710619062,1.,-1.85158945130063));
#29468=CARTESIAN_POINT('Ctrl Pts',(-0.765291664862029,-1.,-1.84553698875924));
#29469=CARTESIAN_POINT('Ctrl Pts',(-0.765291664862029,1.,-1.84553698875924));
#29470=CARTESIAN_POINT('Ctrl Pts',(-0.764978057881737,-1.,-1.83948181064835));
#29471=CARTESIAN_POINT('Ctrl Pts',(-0.764978057881737,1.,-1.83948181064835));
#29472=CARTESIAN_POINT('Ctrl Pts',(-0.764602549687853,-1.,-1.83342077227142));
#29473=CARTESIAN_POINT('Ctrl Pts',(-0.764602549687853,1.,-1.83342077227142));
#29474=CARTESIAN_POINT('Ctrl Pts',(-0.764165902605995,-1.,-1.82735991200065));
#29475=CARTESIAN_POINT('Ctrl Pts',(-0.764165902605995,1.,-1.82735991200065));
#29476=CARTESIAN_POINT('Ctrl Pts',(-0.763673465462726,-1.,-1.82131873145266));
#29477=CARTESIAN_POINT('Ctrl Pts',(-0.763673465462726,1.,-1.82131873145266));
#29478=CARTESIAN_POINT('Ctrl Pts',(-0.763132003836634,-1.,-1.8153211840553));
#29479=CARTESIAN_POINT('Ctrl Pts',(-0.763132003836634,1.,-1.8153211840553));
#29480=CARTESIAN_POINT('Ctrl Pts',(-0.762546129463938,-1.,-1.80938551463965));
#29481=CARTESIAN_POINT('Ctrl Pts',(-0.762546129463938,1.,-1.80938551463965));
#29482=CARTESIAN_POINT('Ctrl Pts',(-0.761915336443547,-1.,-1.80351583877342));
#29483=CARTESIAN_POINT('Ctrl Pts',(-0.761915336443547,1.,-1.80351583877342));
#29484=CARTESIAN_POINT('Ctrl Pts',(-0.761229695230558,-1.,-1.79768986997783));
#29485=CARTESIAN_POINT('Ctrl Pts',(-0.761229695230558,1.,-1.79768986997783));
#29486=CARTESIAN_POINT('Ctrl Pts',(-0.760469555880749,-1.,-1.7918581561088));
#29487=CARTESIAN_POINT('Ctrl Pts',(-0.760469555880749,1.,-1.7918581561088));
#29488=CARTESIAN_POINT('Ctrl Pts',(-0.759614401110189,-1.,-1.78596964884604));
#29489=CARTESIAN_POINT('Ctrl Pts',(-0.759614401110189,1.,-1.78596964884604));
#29490=CARTESIAN_POINT('Ctrl Pts',(-0.758650626677518,-1.,-1.77999411220945));
#29491=CARTESIAN_POINT('Ctrl Pts',(-0.758650626677518,1.,-1.77999411220945));
#29492=CARTESIAN_POINT('Ctrl Pts',(-0.757578264077029,-1.,-1.77394167108292));
#29493=CARTESIAN_POINT('Ctrl Pts',(-0.757578264077029,1.,-1.77394167108292));
#29494=CARTESIAN_POINT('Ctrl Pts',(-0.75642189602781,-1.,-1.76789396002998));
#29495=CARTESIAN_POINT('Ctrl Pts',(-0.75642189602781,1.,-1.76789396002998));
#29496=CARTESIAN_POINT('Ctrl Pts',(-0.755220979974461,-1.,-1.76197817240128));
#29497=CARTESIAN_POINT('Ctrl Pts',(-0.755220979974461,1.,-1.76197817240128));
#29498=CARTESIAN_POINT('Ctrl Pts',(-0.754009254027829,-1.,-1.75631083600019));
#29499=CARTESIAN_POINT('Ctrl Pts',(-0.754009254027829,1.,-1.75631083600019));
#29500=CARTESIAN_POINT('Ctrl Pts',(-0.752797683531314,-1.,-1.75095139468794));
#29501=CARTESIAN_POINT('Ctrl Pts',(-0.752797683531314,1.,-1.75095139468794));
#29502=CARTESIAN_POINT('Ctrl Pts',(-0.751555614164482,-1.,-1.74585086852502));
#29503=CARTESIAN_POINT('Ctrl Pts',(-0.751555614164482,1.,-1.74585086852502));
#29504=CARTESIAN_POINT('Ctrl Pts',(-0.750193435981249,-1.,-1.74080458267114));
#29505=CARTESIAN_POINT('Ctrl Pts',(-0.750193435981249,1.,-1.74080458267114));
#29506=CARTESIAN_POINT('Ctrl Pts',(-0.74858246295687,-1.,-1.7355035168033));
#29507=CARTESIAN_POINT('Ctrl Pts',(-0.74858246295687,1.,-1.7355035168033));
#29508=CARTESIAN_POINT('Ctrl Pts',(-0.746574710097752,-1.,-1.72958533647714));
#29509=CARTESIAN_POINT('Ctrl Pts',(-0.746574710097752,1.,-1.72958533647714));
#29510=CARTESIAN_POINT('Ctrl Pts',(-0.744021445433093,-1.,-1.72268229916769));
#29511=CARTESIAN_POINT('Ctrl Pts',(-0.744021445433093,1.,-1.72268229916769));
#29512=CARTESIAN_POINT('Ctrl Pts',(-0.74079516202821,-1.,-1.71447789751001));
#29513=CARTESIAN_POINT('Ctrl Pts',(-0.74079516202821,1.,-1.71447789751001));
#29514=CARTESIAN_POINT('Ctrl Pts',(-0.736799665716932,-1.,-1.70473309004249));
#29515=CARTESIAN_POINT('Ctrl Pts',(-0.736799665716932,1.,-1.70473309004249));
#29516=CARTESIAN_POINT('Ctrl Pts',(-0.731963238685357,-1.,-1.69326921972915));
#29517=CARTESIAN_POINT('Ctrl Pts',(-0.731963238685357,1.,-1.69326921972915));
#29518=CARTESIAN_POINT('Ctrl Pts',(-0.726235967982445,-1.,-1.67996158451922));
#29519=CARTESIAN_POINT('Ctrl Pts',(-0.726235967982445,1.,-1.67996158451922));
#29520=CARTESIAN_POINT('Ctrl Pts',(-0.71958543378795,-1.,-1.66472880551777));
#29521=CARTESIAN_POINT('Ctrl Pts',(-0.71958543378795,1.,-1.66472880551777));
#29522=CARTESIAN_POINT('Ctrl Pts',(-0.711993139340447,-1.,-1.64752408828442));
#29523=CARTESIAN_POINT('Ctrl Pts',(-0.711993139340447,1.,-1.64752408828442));
#29524=CARTESIAN_POINT('Ctrl Pts',(-0.705159151977294,-1.,-1.6321654166204));
#29525=CARTESIAN_POINT('Ctrl Pts',(-0.705159151977294,1.,-1.6321654166204));
#29526=CARTESIAN_POINT('Ctrl Pts',(-0.699605146398837,-1.,-1.61974673471117));
#29527=CARTESIAN_POINT('Ctrl Pts',(-0.699605146398837,1.,-1.61974673471117));
#29528=CARTESIAN_POINT('Ctrl Pts',(-0.69571209787897,-1.,-1.61106790957619));
#29529=CARTESIAN_POINT('Ctrl Pts',(-0.69571209787897,1.,-1.61106790957619));
#29530=CARTESIAN_POINT('Ctrl Pts',(-0.693717979106305,-1.,-1.60662857109684));
#29531=CARTESIAN_POINT('Ctrl Pts',(-0.693717979106305,1.,-1.60662857109684));
#29532=CARTESIAN_POINT('',(-0.745574324794401,1.,-2.0698113262342));
#29533=CARTESIAN_POINT('Ctrl Pts',(-0.745574324794401,1.,-2.0698113262342));
#29534=CARTESIAN_POINT('Ctrl Pts',(-0.745832791378367,1.,-2.06854248895728));
#29535=CARTESIAN_POINT('Ctrl Pts',(-0.7463458715442,1.,-2.06600523016815));
#29536=CARTESIAN_POINT('Ctrl Pts',(-0.747103932787919,1.,-2.06220058927826));
#29537=CARTESIAN_POINT('Ctrl Pts',(-0.748091554183802,1.,-2.05713023031006));
#29538=CARTESIAN_POINT('Ctrl Pts',(-0.749287468665046,1.,-2.05079645592154));
#29539=CARTESIAN_POINT('Ctrl Pts',(-0.750444657875576,1.,-2.04446689147979));
#29540=CARTESIAN_POINT('Ctrl Pts',(-0.751562963361115,1.,-2.03814160092099));
#29541=CARTESIAN_POINT('Ctrl Pts',(-0.752642180487211,1.,-2.03182068456221));
#29542=CARTESIAN_POINT('Ctrl Pts',(-0.753682061112768,1.,-2.02550428623313));
#29543=CARTESIAN_POINT('Ctrl Pts',(-0.754682330722816,1.,-2.01919259405809));
#29544=CARTESIAN_POINT('Ctrl Pts',(-0.755642704957865,1.,-2.01288584328084));
#29545=CARTESIAN_POINT('Ctrl Pts',(-0.75656290464667,1.,-2.0065843158773));
#29546=CARTESIAN_POINT('Ctrl Pts',(-0.757442676862724,1.,-2.00028834739178));
#29547=CARTESIAN_POINT('Ctrl Pts',(-0.758281796766761,1.,-1.99399831098817));
#29548=CARTESIAN_POINT('Ctrl Pts',(-0.759080037802488,1.,-1.98771456680874));
#29549=CARTESIAN_POINT('Ctrl Pts',(-0.75983714745219,1.,-1.98143741418172));
#29550=CARTESIAN_POINT('Ctrl Pts',(-0.760552825409757,1.,-1.97516705321494));
#29551=CARTESIAN_POINT('Ctrl Pts',(-0.76122669048382,1.,-1.96890351582499));
#29552=CARTESIAN_POINT('Ctrl Pts',(-0.761858300014423,1.,-1.96264672744186));
#29553=CARTESIAN_POINT('Ctrl Pts',(-0.762447203806179,1.,-1.95639665309869));
#29554=CARTESIAN_POINT('Ctrl Pts',(-0.762992990878769,1.,-1.95015342590024));
#29555=CARTESIAN_POINT('Ctrl Pts',(-0.763495333538629,1.,-1.9439174661764));
#29556=CARTESIAN_POINT('Ctrl Pts',(-0.763954049121458,1.,-1.93768964875886));
#29557=CARTESIAN_POINT('Ctrl Pts',(-0.764369010673941,1.,-1.93147105496382));
#29558=CARTESIAN_POINT('Ctrl Pts',(-0.764740025488211,1.,-1.92526263537048));
#29559=CARTESIAN_POINT('Ctrl Pts',(-0.765066729667088,1.,-1.91906491634196));
#29560=CARTESIAN_POINT('Ctrl Pts',(-0.765348465884722,1.,-1.91287765805169));
#29561=CARTESIAN_POINT('Ctrl Pts',(-0.765584196937919,1.,-1.90669961402356));
#29562=CARTESIAN_POINT('Ctrl Pts',(-0.765772772593386,1.,-1.90052930393596));
#29563=CARTESIAN_POINT('Ctrl Pts',(-0.765913193856978,1.,-1.89436577771388));
#29564=CARTESIAN_POINT('Ctrl Pts',(-0.766004837062091,1.,-1.88820926433409));
#29565=CARTESIAN_POINT('Ctrl Pts',(-0.766047794851865,1.,-1.88206215302561));
#29566=CARTESIAN_POINT('Ctrl Pts',(-0.766042837036744,1.,-1.87592888967883));
#29567=CARTESIAN_POINT('Ctrl Pts',(-0.765990708546091,1.,-1.86981398314341));
#29568=CARTESIAN_POINT('Ctrl Pts',(-0.765891519092547,1.,-1.86372027063312));
#29569=CARTESIAN_POINT('Ctrl Pts',(-0.765744212909318,1.,-1.85764741390394));
#29570=CARTESIAN_POINT('Ctrl Pts',(-0.765545710619062,1.,-1.85158945130063));
#29571=CARTESIAN_POINT('Ctrl Pts',(-0.765291664862029,1.,-1.84553698875924));
#29572=CARTESIAN_POINT('Ctrl Pts',(-0.764978057881737,1.,-1.83948181064835));
#29573=CARTESIAN_POINT('Ctrl Pts',(-0.764602549687853,1.,-1.83342077227142));
#29574=CARTESIAN_POINT('Ctrl Pts',(-0.764165902605995,1.,-1.82735991200065));
#29575=CARTESIAN_POINT('Ctrl Pts',(-0.763673465462726,1.,-1.82131873145266));
#29576=CARTESIAN_POINT('Ctrl Pts',(-0.763132003836634,1.,-1.8153211840553));
#29577=CARTESIAN_POINT('Ctrl Pts',(-0.762546129463938,1.,-1.80938551463965));
#29578=CARTESIAN_POINT('Ctrl Pts',(-0.761915336443547,1.,-1.80351583877342));
#29579=CARTESIAN_POINT('Ctrl Pts',(-0.761229695230558,1.,-1.79768986997783));
#29580=CARTESIAN_POINT('Ctrl Pts',(-0.760469555880749,1.,-1.7918581561088));
#29581=CARTESIAN_POINT('Ctrl Pts',(-0.759614401110189,1.,-1.78596964884604));
#29582=CARTESIAN_POINT('Ctrl Pts',(-0.758650626677518,1.,-1.77999411220945));
#29583=CARTESIAN_POINT('Ctrl Pts',(-0.757578264077029,1.,-1.77394167108292));
#29584=CARTESIAN_POINT('Ctrl Pts',(-0.75642189602781,1.,-1.76789396002998));
#29585=CARTESIAN_POINT('Ctrl Pts',(-0.755220979974461,1.,-1.76197817240128));
#29586=CARTESIAN_POINT('Ctrl Pts',(-0.754009254027829,1.,-1.75631083600019));
#29587=CARTESIAN_POINT('Ctrl Pts',(-0.752797683531314,1.,-1.75095139468794));
#29588=CARTESIAN_POINT('Ctrl Pts',(-0.751555614164482,1.,-1.74585086852502));
#29589=CARTESIAN_POINT('Ctrl Pts',(-0.750193435981249,1.,-1.74080458267114));
#29590=CARTESIAN_POINT('Ctrl Pts',(-0.74858246295687,1.,-1.7355035168033));
#29591=CARTESIAN_POINT('Ctrl Pts',(-0.746574710097752,1.,-1.72958533647714));
#29592=CARTESIAN_POINT('Ctrl Pts',(-0.744021445433093,1.,-1.72268229916769));
#29593=CARTESIAN_POINT('Ctrl Pts',(-0.74079516202821,1.,-1.71447789751001));
#29594=CARTESIAN_POINT('Ctrl Pts',(-0.736799665716932,1.,-1.70473309004249));
#29595=CARTESIAN_POINT('Ctrl Pts',(-0.731963238685357,1.,-1.69326921972915));
#29596=CARTESIAN_POINT('Ctrl Pts',(-0.726235967982445,1.,-1.67996158451922));
#29597=CARTESIAN_POINT('Ctrl Pts',(-0.71958543378795,1.,-1.66472880551777));
#29598=CARTESIAN_POINT('Ctrl Pts',(-0.711993139340447,1.,-1.64752408828442));
#29599=CARTESIAN_POINT('Ctrl Pts',(-0.705159151977294,1.,-1.6321654166204));
#29600=CARTESIAN_POINT('Ctrl Pts',(-0.699605146398837,1.,-1.61974673471117));
#29601=CARTESIAN_POINT('Ctrl Pts',(-0.69571209787897,1.,-1.61106790957619));
#29602=CARTESIAN_POINT('Ctrl Pts',(-0.693717979106305,1.,-1.60662857109684));
#29603=CARTESIAN_POINT('',(-0.745574324794401,0.,-2.0698113262342));
#29604=CARTESIAN_POINT('Origin',(-0.61342227326009,0.,-2.11275013067528));
#29605=CARTESIAN_POINT('',(-0.61342227326009,1.,-2.11275013067528));
#29606=CARTESIAN_POINT('',(-0.745574324794401,1.,-2.0698113262342));
#29607=CARTESIAN_POINT('',(-0.61342227326009,0.,-2.11275013067528));
#29608=CARTESIAN_POINT('Ctrl Pts',(-0.383122945602004,-1.,-1.7075470150345));
#29609=CARTESIAN_POINT('Ctrl Pts',(-0.383122945602004,1.,-1.7075470150345));
#29610=CARTESIAN_POINT('Ctrl Pts',(-0.384119047315542,-1.,-1.71231062891958));
#29611=CARTESIAN_POINT('Ctrl Pts',(-0.384119047315542,1.,-1.71231062891958));
#29612=CARTESIAN_POINT('Ctrl Pts',(-0.38607079032701,-1.,-1.72162022246158));
#29613=CARTESIAN_POINT('Ctrl Pts',(-0.38607079032701,1.,-1.72162022246158));
#29614=CARTESIAN_POINT('Ctrl Pts',(-0.388877023509191,-1.,-1.7349317097561));
#29615=CARTESIAN_POINT('Ctrl Pts',(-0.388877023509191,1.,-1.7349317097561));
#29616=CARTESIAN_POINT('Ctrl Pts',(-0.392375812294307,-1.,-1.75137405313962));
#29617=CARTESIAN_POINT('Ctrl Pts',(-0.392375812294307,1.,-1.75137405313962));
#29618=CARTESIAN_POINT('Ctrl Pts',(-0.39634619612042,-1.,-1.7697556004756));
#29619=CARTESIAN_POINT('Ctrl Pts',(-0.39634619612042,1.,-1.7697556004756));
#29620=CARTESIAN_POINT('Ctrl Pts',(-0.39991940378308,-1.,-1.78598826347533));
#29621=CARTESIAN_POINT('Ctrl Pts',(-0.39991940378308,1.,-1.78598826347533));
#29622=CARTESIAN_POINT('Ctrl Pts',(-0.403107976170441,-1.,-1.80012077176221));
#29623=CARTESIAN_POINT('Ctrl Pts',(-0.403107976170441,1.,-1.80012077176221));
#29624=CARTESIAN_POINT('Ctrl Pts',(-0.405933518411838,-1.,-1.81223801813988));
#29625=CARTESIAN_POINT('Ctrl Pts',(-0.405933518411838,1.,-1.81223801813988));
#29626=CARTESIAN_POINT('Ctrl Pts',(-0.408428948108533,-1.,-1.8224702267854));
#29627=CARTESIAN_POINT('Ctrl Pts',(-0.408428948108533,1.,-1.8224702267854));
#29628=CARTESIAN_POINT('Ctrl Pts',(-0.410641256301675,-1.,-1.83100408895216));
#29629=CARTESIAN_POINT('Ctrl Pts',(-0.410641256301675,1.,-1.83100408895216));
#29630=CARTESIAN_POINT('Ctrl Pts',(-0.412633125322162,-1.,-1.83808953475839));
#29631=CARTESIAN_POINT('Ctrl Pts',(-0.412633125322162,1.,-1.83808953475839));
#29632=CARTESIAN_POINT('Ctrl Pts',(-0.41448743825434,-1.,-1.8440575707371));
#29633=CARTESIAN_POINT('Ctrl Pts',(-0.41448743825434,1.,-1.8440575707371));
#29634=CARTESIAN_POINT('Ctrl Pts',(-0.416300022038864,-1.,-1.84929312929882));
#29635=CARTESIAN_POINT('Ctrl Pts',(-0.416300022038864,1.,-1.84929312929882));
#29636=CARTESIAN_POINT('Ctrl Pts',(-0.418164129143534,-1.,-1.85417632856234));
#29637=CARTESIAN_POINT('Ctrl Pts',(-0.418164129143534,1.,-1.85417632856234));
#29638=CARTESIAN_POINT('Ctrl Pts',(-0.420157287975619,-1.,-1.85903281096686));
#29639=CARTESIAN_POINT('Ctrl Pts',(-0.420157287975619,1.,-1.85903281096686));
#29640=CARTESIAN_POINT('Ctrl Pts',(-0.422327307418275,-1.,-1.86408083334028));
#29641=CARTESIAN_POINT('Ctrl Pts',(-0.422327307418275,1.,-1.86408083334028));
#29642=CARTESIAN_POINT('Ctrl Pts',(-0.424678177291359,-1.,-1.86937803944323));
#29643=CARTESIAN_POINT('Ctrl Pts',(-0.424678177291359,1.,-1.86937803944323));
#29644=CARTESIAN_POINT('Ctrl Pts',(-0.427183828519102,-1.,-1.87486989291484));
#29645=CARTESIAN_POINT('Ctrl Pts',(-0.427183828519102,1.,-1.87486989291484));
#29646=CARTESIAN_POINT('Ctrl Pts',(-0.429803062482344,-1.,-1.88044229001832));
#29647=CARTESIAN_POINT('Ctrl Pts',(-0.429803062482344,1.,-1.88044229001832));
#29648=CARTESIAN_POINT('Ctrl Pts',(-0.432493038548748,-1.,-1.88596913666793));
#29649=CARTESIAN_POINT('Ctrl Pts',(-0.432493038548748,1.,-1.88596913666793));
#29650=CARTESIAN_POINT('Ctrl Pts',(-0.435225660963383,-1.,-1.89136993975504));
#29651=CARTESIAN_POINT('Ctrl Pts',(-0.435225660963383,1.,-1.89136993975504));
#29652=CARTESIAN_POINT('Ctrl Pts',(-0.437995003948244,-1.,-1.89663648956466));
#29653=CARTESIAN_POINT('Ctrl Pts',(-0.437995003948244,1.,-1.89663648956466));
#29654=CARTESIAN_POINT('Ctrl Pts',(-0.440807833704038,-1.,-1.90180124389086));
#29655=CARTESIAN_POINT('Ctrl Pts',(-0.440807833704038,1.,-1.90180124389086));
#29656=CARTESIAN_POINT('Ctrl Pts',(-0.443677556849151,-1.,-1.90691756144898));
#29657=CARTESIAN_POINT('Ctrl Pts',(-0.443677556849151,1.,-1.90691756144898));
#29658=CARTESIAN_POINT('Ctrl Pts',(-0.446617343485711,-1.,-1.9120369998112));
#29659=CARTESIAN_POINT('Ctrl Pts',(-0.446617343485711,1.,-1.9120369998112));
#29660=CARTESIAN_POINT('Ctrl Pts',(-0.449632260106662,-1.,-1.91718342555755));
#29661=CARTESIAN_POINT('Ctrl Pts',(-0.449632260106662,1.,-1.91718342555755));
#29662=CARTESIAN_POINT('Ctrl Pts',(-0.452719478359432,-1.,-1.92235380648502));
#29663=CARTESIAN_POINT('Ctrl Pts',(-0.452719478359432,1.,-1.92235380648502));
#29664=CARTESIAN_POINT('Ctrl Pts',(-0.455872005174371,-1.,-1.92753067150476));
#29665=CARTESIAN_POINT('Ctrl Pts',(-0.455872005174371,1.,-1.92753067150476));
#29666=CARTESIAN_POINT('Ctrl Pts',(-0.459081234547926,-1.,-1.93269066517934));
#29667=CARTESIAN_POINT('Ctrl Pts',(-0.459081234547926,1.,-1.93269066517934));
#29668=CARTESIAN_POINT('Ctrl Pts',(-0.462340031009056,-1.,-1.93781486640821));
#29669=CARTESIAN_POINT('Ctrl Pts',(-0.462340031009056,1.,-1.93781486640821));
#29670=CARTESIAN_POINT('Ctrl Pts',(-0.46564546202603,-1.,-1.9428979419619));
#29671=CARTESIAN_POINT('Ctrl Pts',(-0.46564546202603,1.,-1.9428979419619));
#29672=CARTESIAN_POINT('Ctrl Pts',(-0.468997482913135,-1.,-1.94794381136514));
#29673=CARTESIAN_POINT('Ctrl Pts',(-0.468997482913135,1.,-1.94794381136514));
#29674=CARTESIAN_POINT('Ctrl Pts',(-0.472397672264072,-1.,-1.95296148278133));
#29675=CARTESIAN_POINT('Ctrl Pts',(-0.472397672264072,1.,-1.95296148278133));
#29676=CARTESIAN_POINT('Ctrl Pts',(-0.475848034683176,-1.,-1.95796111148177));
#29677=CARTESIAN_POINT('Ctrl Pts',(-0.475848034683176,1.,-1.95796111148177));
#29678=CARTESIAN_POINT('Ctrl Pts',(-0.479349583074855,-1.,-1.96294933055943));
#29679=CARTESIAN_POINT('Ctrl Pts',(-0.479349583074855,1.,-1.96294933055943));
#29680=CARTESIAN_POINT('Ctrl Pts',(-0.482901662120691,-1.,-1.96792703422362));
#29681=CARTESIAN_POINT('Ctrl Pts',(-0.482901662120691,1.,-1.96792703422362));
#29682=CARTESIAN_POINT('Ctrl Pts',(-0.486502692907659,-1.,-1.97289186263272));
#29683=CARTESIAN_POINT('Ctrl Pts',(-0.486502692907659,1.,-1.97289186263272));
#29684=CARTESIAN_POINT('Ctrl Pts',(-0.490150627860952,-1.,-1.97783973019229));
#29685=CARTESIAN_POINT('Ctrl Pts',(-0.490150627860952,1.,-1.97783973019229));
#29686=CARTESIAN_POINT('Ctrl Pts',(-0.493843476541495,-1.,-1.98276658761821));
#29687=CARTESIAN_POINT('Ctrl Pts',(-0.493843476541495,1.,-1.98276658761821));
#29688=CARTESIAN_POINT('Ctrl Pts',(-0.497579909545574,-1.,-1.98767044752932));
#29689=CARTESIAN_POINT('Ctrl Pts',(-0.497579909545574,1.,-1.98767044752932));
#29690=CARTESIAN_POINT('Ctrl Pts',(-0.501359287727146,-1.,-1.99255149126155));
#29691=CARTESIAN_POINT('Ctrl Pts',(-0.501359287727146,1.,-1.99255149126155));
#29692=CARTESIAN_POINT('Ctrl Pts',(-0.505181361323026,-1.,-1.99741107463572));
#29693=CARTESIAN_POINT('Ctrl Pts',(-0.505181361323026,1.,-1.99741107463572));
#29694=CARTESIAN_POINT('Ctrl Pts',(-0.509046069886157,-1.,-2.00225107134734));
#29695=CARTESIAN_POINT('Ctrl Pts',(-0.509046069886157,1.,-2.00225107134734));
#29696=CARTESIAN_POINT('Ctrl Pts',(-0.512953306961792,-1.,-2.00707309946949));
#29697=CARTESIAN_POINT('Ctrl Pts',(-0.512953306961792,1.,-2.00707309946949));
#29698=CARTESIAN_POINT('Ctrl Pts',(-0.516902681728687,-1.,-2.01187773939242));
#29699=CARTESIAN_POINT('Ctrl Pts',(-0.516902681728687,1.,-2.01187773939242));
#29700=CARTESIAN_POINT('Ctrl Pts',(-0.52089359039937,-1.,-2.01666477917286));
#29701=CARTESIAN_POINT('Ctrl Pts',(-0.52089359039937,1.,-2.01666477917286));
#29702=CARTESIAN_POINT('Ctrl Pts',(-0.524925318333476,-1.,-2.02143356304698));
#29703=CARTESIAN_POINT('Ctrl Pts',(-0.524925318333476,1.,-2.02143356304698));
#29704=CARTESIAN_POINT('Ctrl Pts',(-0.528997127241914,-1.,-2.0261832908329));
#29705=CARTESIAN_POINT('Ctrl Pts',(-0.528997127241914,1.,-2.0261832908329));
#29706=CARTESIAN_POINT('Ctrl Pts',(-0.533108355132977,-1.,-2.03091336214426));
#29707=CARTESIAN_POINT('Ctrl Pts',(-0.533108355132977,1.,-2.03091336214426));
#29708=CARTESIAN_POINT('Ctrl Pts',(-0.537258489833262,-1.,-2.03562362954037));
#29709=CARTESIAN_POINT('Ctrl Pts',(-0.537258489833262,1.,-2.03562362954037));
#29710=CARTESIAN_POINT('Ctrl Pts',(-0.541447120615659,-1.,-2.04031422690527));
#29711=CARTESIAN_POINT('Ctrl Pts',(-0.541447120615659,1.,-2.04031422690527));
#29712=CARTESIAN_POINT('Ctrl Pts',(-0.54567390381743,-1.,-2.04498544714588));
#29713=CARTESIAN_POINT('Ctrl Pts',(-0.54567390381743,1.,-2.04498544714588));
#29714=CARTESIAN_POINT('Ctrl Pts',(-0.549938525150295,-1.,-2.04963761077958));
#29715=CARTESIAN_POINT('Ctrl Pts',(-0.549938525150295,1.,-2.04963761077958));
#29716=CARTESIAN_POINT('Ctrl Pts',(-0.554240657463906,-1.,-2.05427091604413));
#29717=CARTESIAN_POINT('Ctrl Pts',(-0.554240657463906,1.,-2.05427091604413));
#29718=CARTESIAN_POINT('Ctrl Pts',(-0.558579940185151,-1.,-2.05888537756462));
#29719=CARTESIAN_POINT('Ctrl Pts',(-0.558579940185151,1.,-2.05888537756462));
#29720=CARTESIAN_POINT('Ctrl Pts',(-0.562955993082261,-1.,-2.06348090160589));
#29721=CARTESIAN_POINT('Ctrl Pts',(-0.562955993082261,1.,-2.06348090160589));
#29722=CARTESIAN_POINT('Ctrl Pts',(-0.567368421181087,-1.,-2.06805732997334));
#29723=CARTESIAN_POINT('Ctrl Pts',(-0.567368421181087,1.,-2.06805732997334));
#29724=CARTESIAN_POINT('Ctrl Pts',(-0.571816823242603,-1.,-2.07261449292824));
#29725=CARTESIAN_POINT('Ctrl Pts',(-0.571816823242603,1.,-2.07261449292824));
#29726=CARTESIAN_POINT('Ctrl Pts',(-0.576300797416844,-1.,-2.07715226767559));
#29727=CARTESIAN_POINT('Ctrl Pts',(-0.576300797416844,1.,-2.07715226767559));
#29728=CARTESIAN_POINT('Ctrl Pts',(-0.580819952108063,-1.,-2.08167059018418));
#29729=CARTESIAN_POINT('Ctrl Pts',(-0.580819952108063,1.,-2.08167059018418));
#29730=CARTESIAN_POINT('Ctrl Pts',(-0.585373918991617,-1.,-2.08616943727951));
#29731=CARTESIAN_POINT('Ctrl Pts',(-0.585373918991617,1.,-2.08616943727951));
#29732=CARTESIAN_POINT('Ctrl Pts',(-0.589962365403406,-1.,-2.09064881812129));
#29733=CARTESIAN_POINT('Ctrl Pts',(-0.589962365403406,1.,-2.09064881812129));
#29734=CARTESIAN_POINT('Ctrl Pts',(-0.594585006052162,-1.,-2.0951087622027));
#29735=CARTESIAN_POINT('Ctrl Pts',(-0.594585006052162,1.,-2.0951087622027));
#29736=CARTESIAN_POINT('Ctrl Pts',(-0.599241616420533,-1.,-2.0995493086477));
#29737=CARTESIAN_POINT('Ctrl Pts',(-0.599241616420533,1.,-2.0995493086477));
#29738=CARTESIAN_POINT('Ctrl Pts',(-0.60393203073603,-1.,-2.10397049886949));
#29739=CARTESIAN_POINT('Ctrl Pts',(-0.60393203073603,1.,-2.10397049886949));
#29740=CARTESIAN_POINT('Ctrl Pts',(-0.607711315454876,-1.,-2.1074919961518));
#29741=CARTESIAN_POINT('Ctrl Pts',(-0.607711315454876,1.,-2.1074919961518));
#29742=CARTESIAN_POINT('Ctrl Pts',(-0.610560911689899,-1.,-2.11012443807238));
#29743=CARTESIAN_POINT('Ctrl Pts',(-0.610560911689899,1.,-2.11012443807238));
#29744=CARTESIAN_POINT('Ctrl Pts',(-0.6124673655618,-1.,-2.11187554259986));
#29745=CARTESIAN_POINT('Ctrl Pts',(-0.6124673655618,1.,-2.11187554259986));
#29746=CARTESIAN_POINT('Ctrl Pts',(-0.61342227326009,-1.,-2.11275013067528));
#29747=CARTESIAN_POINT('Ctrl Pts',(-0.61342227326009,1.,-2.11275013067528));
#29748=CARTESIAN_POINT('',(-0.383122945602004,1.,-1.7075470150345));
#29749=CARTESIAN_POINT('Ctrl Pts',(-0.383122945602004,1.,-1.7075470150345));
#29750=CARTESIAN_POINT('Ctrl Pts',(-0.384119047315542,1.,-1.71231062891958));
#29751=CARTESIAN_POINT('Ctrl Pts',(-0.38607079032701,1.,-1.72162022246158));
#29752=CARTESIAN_POINT('Ctrl Pts',(-0.388877023509191,1.,-1.7349317097561));
#29753=CARTESIAN_POINT('Ctrl Pts',(-0.392375812294307,1.,-1.75137405313962));
#29754=CARTESIAN_POINT('Ctrl Pts',(-0.39634619612042,1.,-1.7697556004756));
#29755=CARTESIAN_POINT('Ctrl Pts',(-0.39991940378308,1.,-1.78598826347533));
#29756=CARTESIAN_POINT('Ctrl Pts',(-0.403107976170441,1.,-1.80012077176221));
#29757=CARTESIAN_POINT('Ctrl Pts',(-0.405933518411838,1.,-1.81223801813988));
#29758=CARTESIAN_POINT('Ctrl Pts',(-0.408428948108533,1.,-1.8224702267854));
#29759=CARTESIAN_POINT('Ctrl Pts',(-0.410641256301675,1.,-1.83100408895216));
#29760=CARTESIAN_POINT('Ctrl Pts',(-0.412633125322162,1.,-1.83808953475839));
#29761=CARTESIAN_POINT('Ctrl Pts',(-0.41448743825434,1.,-1.8440575707371));
#29762=CARTESIAN_POINT('Ctrl Pts',(-0.416300022038864,1.,-1.84929312929882));
#29763=CARTESIAN_POINT('Ctrl Pts',(-0.418164129143534,1.,-1.85417632856234));
#29764=CARTESIAN_POINT('Ctrl Pts',(-0.420157287975619,1.,-1.85903281096686));
#29765=CARTESIAN_POINT('Ctrl Pts',(-0.422327307418275,1.,-1.86408083334028));
#29766=CARTESIAN_POINT('Ctrl Pts',(-0.424678177291359,1.,-1.86937803944323));
#29767=CARTESIAN_POINT('Ctrl Pts',(-0.427183828519102,1.,-1.87486989291484));
#29768=CARTESIAN_POINT('Ctrl Pts',(-0.429803062482344,1.,-1.88044229001832));
#29769=CARTESIAN_POINT('Ctrl Pts',(-0.432493038548748,1.,-1.88596913666793));
#29770=CARTESIAN_POINT('Ctrl Pts',(-0.435225660963383,1.,-1.89136993975504));
#29771=CARTESIAN_POINT('Ctrl Pts',(-0.437995003948244,1.,-1.89663648956466));
#29772=CARTESIAN_POINT('Ctrl Pts',(-0.440807833704038,1.,-1.90180124389086));
#29773=CARTESIAN_POINT('Ctrl Pts',(-0.443677556849151,1.,-1.90691756144898));
#29774=CARTESIAN_POINT('Ctrl Pts',(-0.446617343485711,1.,-1.9120369998112));
#29775=CARTESIAN_POINT('Ctrl Pts',(-0.449632260106662,1.,-1.91718342555755));
#29776=CARTESIAN_POINT('Ctrl Pts',(-0.452719478359432,1.,-1.92235380648502));
#29777=CARTESIAN_POINT('Ctrl Pts',(-0.455872005174371,1.,-1.92753067150476));
#29778=CARTESIAN_POINT('Ctrl Pts',(-0.459081234547926,1.,-1.93269066517934));
#29779=CARTESIAN_POINT('Ctrl Pts',(-0.462340031009056,1.,-1.93781486640821));
#29780=CARTESIAN_POINT('Ctrl Pts',(-0.46564546202603,1.,-1.9428979419619));
#29781=CARTESIAN_POINT('Ctrl Pts',(-0.468997482913135,1.,-1.94794381136514));
#29782=CARTESIAN_POINT('Ctrl Pts',(-0.472397672264072,1.,-1.95296148278133));
#29783=CARTESIAN_POINT('Ctrl Pts',(-0.475848034683176,1.,-1.95796111148177));
#29784=CARTESIAN_POINT('Ctrl Pts',(-0.479349583074855,1.,-1.96294933055943));
#29785=CARTESIAN_POINT('Ctrl Pts',(-0.482901662120691,1.,-1.96792703422362));
#29786=CARTESIAN_POINT('Ctrl Pts',(-0.486502692907659,1.,-1.97289186263272));
#29787=CARTESIAN_POINT('Ctrl Pts',(-0.490150627860952,1.,-1.97783973019229));
#29788=CARTESIAN_POINT('Ctrl Pts',(-0.493843476541495,1.,-1.98276658761821));
#29789=CARTESIAN_POINT('Ctrl Pts',(-0.497579909545574,1.,-1.98767044752932));
#29790=CARTESIAN_POINT('Ctrl Pts',(-0.501359287727146,1.,-1.99255149126155));
#29791=CARTESIAN_POINT('Ctrl Pts',(-0.505181361323026,1.,-1.99741107463572));
#29792=CARTESIAN_POINT('Ctrl Pts',(-0.509046069886157,1.,-2.00225107134734));
#29793=CARTESIAN_POINT('Ctrl Pts',(-0.512953306961792,1.,-2.00707309946949));
#29794=CARTESIAN_POINT('Ctrl Pts',(-0.516902681728687,1.,-2.01187773939242));
#29795=CARTESIAN_POINT('Ctrl Pts',(-0.52089359039937,1.,-2.01666477917286));
#29796=CARTESIAN_POINT('Ctrl Pts',(-0.524925318333476,1.,-2.02143356304698));
#29797=CARTESIAN_POINT('Ctrl Pts',(-0.528997127241914,1.,-2.0261832908329));
#29798=CARTESIAN_POINT('Ctrl Pts',(-0.533108355132977,1.,-2.03091336214426));
#29799=CARTESIAN_POINT('Ctrl Pts',(-0.537258489833262,1.,-2.03562362954037));
#29800=CARTESIAN_POINT('Ctrl Pts',(-0.541447120615659,1.,-2.04031422690527));
#29801=CARTESIAN_POINT('Ctrl Pts',(-0.54567390381743,1.,-2.04498544714588));
#29802=CARTESIAN_POINT('Ctrl Pts',(-0.549938525150295,1.,-2.04963761077958));
#29803=CARTESIAN_POINT('Ctrl Pts',(-0.554240657463906,1.,-2.05427091604413));
#29804=CARTESIAN_POINT('Ctrl Pts',(-0.558579940185151,1.,-2.05888537756462));
#29805=CARTESIAN_POINT('Ctrl Pts',(-0.562955993082261,1.,-2.06348090160589));
#29806=CARTESIAN_POINT('Ctrl Pts',(-0.567368421181087,1.,-2.06805732997334));
#29807=CARTESIAN_POINT('Ctrl Pts',(-0.571816823242603,1.,-2.07261449292824));
#29808=CARTESIAN_POINT('Ctrl Pts',(-0.576300797416844,1.,-2.07715226767559));
#29809=CARTESIAN_POINT('Ctrl Pts',(-0.580819952108063,1.,-2.08167059018418));
#29810=CARTESIAN_POINT('Ctrl Pts',(-0.585373918991617,1.,-2.08616943727951));
#29811=CARTESIAN_POINT('Ctrl Pts',(-0.589962365403406,1.,-2.09064881812129));
#29812=CARTESIAN_POINT('Ctrl Pts',(-0.594585006052162,1.,-2.0951087622027));
#29813=CARTESIAN_POINT('Ctrl Pts',(-0.599241616420533,1.,-2.0995493086477));
#29814=CARTESIAN_POINT('Ctrl Pts',(-0.60393203073603,1.,-2.10397049886949));
#29815=CARTESIAN_POINT('Ctrl Pts',(-0.607711315454876,1.,-2.1074919961518));
#29816=CARTESIAN_POINT('Ctrl Pts',(-0.610560911689899,1.,-2.11012443807238));
#29817=CARTESIAN_POINT('Ctrl Pts',(-0.6124673655618,1.,-2.11187554259986));
#29818=CARTESIAN_POINT('Ctrl Pts',(-0.61342227326009,1.,-2.11275013067528));
#29819=CARTESIAN_POINT('',(-0.383122945602003,0.,-1.7075470150345));
#29820=CARTESIAN_POINT('Origin',(0.,0.,0.));
#29821=CARTESIAN_POINT('',(-0.163289472382896,1.,-1.74236521665491));
#29822=CARTESIAN_POINT('Origin',(0.,1.,0.));
#29823=CARTESIAN_POINT('',(-0.163289472382896,0.,-1.74236521665491));
#29824=CARTESIAN_POINT('Ctrl Pts',(-0.0694764450219581,-1.,-2.19890268624765));
#29825=CARTESIAN_POINT('Ctrl Pts',(-0.0694764450219581,1.,-2.19890268624765));
#29826=CARTESIAN_POINT('Ctrl Pts',(-0.070114353632549,-1.,-2.19777582085423));
#29827=CARTESIAN_POINT('Ctrl Pts',(-0.070114353632549,1.,-2.19777582085423));
#29828=CARTESIAN_POINT('Ctrl Pts',(-0.0713863779526154,-1.,-2.19552129484002));
#29829=CARTESIAN_POINT('Ctrl Pts',(-0.0713863779526154,1.,-2.19552129484002));
#29830=CARTESIAN_POINT('Ctrl Pts',(-0.0732830357306725,-1.,-2.19213712013662));
#29831=CARTESIAN_POINT('Ctrl Pts',(-0.0732830357306725,1.,-2.19213712013662));
#29832=CARTESIAN_POINT('Ctrl Pts',(-0.0757891465836148,-1.,-2.1876201139953));
#29833=CARTESIAN_POINT('Ctrl Pts',(-0.0757891465836148,1.,-2.1876201139953));
#29834=CARTESIAN_POINT('Ctrl Pts',(-0.0788837727685243,-1.,-2.18196589448887));
#29835=CARTESIAN_POINT('Ctrl Pts',(-0.0788837727685243,1.,-2.18196589448887));
#29836=CARTESIAN_POINT('Ctrl Pts',(-0.0819402680872765,-1.,-2.176303712113));
#29837=CARTESIAN_POINT('Ctrl Pts',(-0.0819402680872765,1.,-2.176303712113));
#29838=CARTESIAN_POINT('Ctrl Pts',(-0.0849584620835372,-1.,-2.17063357870952));
#29839=CARTESIAN_POINT('Ctrl Pts',(-0.0849584620835372,1.,-2.17063357870952));
#29840=CARTESIAN_POINT('Ctrl Pts',(-0.0879381291386923,-1.,-2.16495552645014));
#29841=CARTESIAN_POINT('Ctrl Pts',(-0.0879381291386923,1.,-2.16495552645014));
#29842=CARTESIAN_POINT('Ctrl Pts',(-0.0908789888107265,-1.,-2.15926961544516));
#29843=CARTESIAN_POINT('Ctrl Pts',(-0.0908789888107265,1.,-2.15926961544516));
#29844=CARTESIAN_POINT('Ctrl Pts',(-0.0937807218867643,-1.,-2.1535759397817));
#29845=CARTESIAN_POINT('Ctrl Pts',(-0.0937807218867643,1.,-2.1535759397817));
#29846=CARTESIAN_POINT('Ctrl Pts',(-0.0966429852305459,-1.,-2.14787463531795));
#29847=CARTESIAN_POINT('Ctrl Pts',(-0.0966429852305459,1.,-2.14787463531795));
#29848=CARTESIAN_POINT('Ctrl Pts',(-0.0994654261990915,-1.,-2.14216588396025));
#29849=CARTESIAN_POINT('Ctrl Pts',(-0.0994654261990915,1.,-2.14216588396025));
#29850=CARTESIAN_POINT('Ctrl Pts',(-0.1022477005561,-1.,-2.13644992667165));
#29851=CARTESIAN_POINT('Ctrl Pts',(-0.1022477005561,1.,-2.13644992667165));
#29852=CARTESIAN_POINT('Ctrl Pts',(-0.104989479152739,-1.,-2.13072704887293));
#29853=CARTESIAN_POINT('Ctrl Pts',(-0.104989479152739,1.,-2.13072704887293));
#29854=CARTESIAN_POINT('Ctrl Pts',(-0.10769043523109,-1.,-2.12499752307));
#29855=CARTESIAN_POINT('Ctrl Pts',(-0.10769043523109,1.,-2.12499752307));
#29856=CARTESIAN_POINT('Ctrl Pts',(-0.110350236135025,-1.,-2.11926155590865));
#29857=CARTESIAN_POINT('Ctrl Pts',(-0.110350236135025,1.,-2.11926155590865));
#29858=CARTESIAN_POINT('Ctrl Pts',(-0.112968534419737,-1.,-2.11351924490306));
#29859=CARTESIAN_POINT('Ctrl Pts',(-0.112968534419737,1.,-2.11351924490306));
#29860=CARTESIAN_POINT('Ctrl Pts',(-0.115544957687926,-1.,-2.10777050261309));
#29861=CARTESIAN_POINT('Ctrl Pts',(-0.115544957687926,1.,-2.10777050261309));
#29862=CARTESIAN_POINT('Ctrl Pts',(-0.118079107988355,-1.,-2.102015121329));
#29863=CARTESIAN_POINT('Ctrl Pts',(-0.118079107988355,1.,-2.102015121329));
#29864=CARTESIAN_POINT('Ctrl Pts',(-0.120570567965122,-1.,-2.0962529286773));
#29865=CARTESIAN_POINT('Ctrl Pts',(-0.120570567965122,1.,-2.0962529286773));
#29866=CARTESIAN_POINT('Ctrl Pts',(-0.123018905621083,-1.,-2.09048392424825));
#29867=CARTESIAN_POINT('Ctrl Pts',(-0.123018905621083,1.,-2.09048392424825));
#29868=CARTESIAN_POINT('Ctrl Pts',(-0.125423679412061,-1.,-2.08470840653643));
#29869=CARTESIAN_POINT('Ctrl Pts',(-0.125423679412061,1.,-2.08470840653643));
#29870=CARTESIAN_POINT('Ctrl Pts',(-0.12778444527612,-1.,-2.07892715110987));
#29871=CARTESIAN_POINT('Ctrl Pts',(-0.12778444527612,1.,-2.07892715110987));
#29872=CARTESIAN_POINT('Ctrl Pts',(-0.130100748328403,-1.,-2.07314114713063));
#29873=CARTESIAN_POINT('Ctrl Pts',(-0.130100748328403,1.,-2.07314114713063));
#29874=CARTESIAN_POINT('Ctrl Pts',(-0.13237211154771,-1.,-2.06735123910326));
#29875=CARTESIAN_POINT('Ctrl Pts',(-0.13237211154771,1.,-2.06735123910326));
#29876=CARTESIAN_POINT('Ctrl Pts',(-0.134598026192106,-1.,-2.06155781517842));
#29877=CARTESIAN_POINT('Ctrl Pts',(-0.134598026192106,1.,-2.06155781517842));
#29878=CARTESIAN_POINT('Ctrl Pts',(-0.136777941218044,-1.,-2.05576044414264));
#29879=CARTESIAN_POINT('Ctrl Pts',(-0.136777941218044,1.,-2.05576044414264));
#29880=CARTESIAN_POINT('Ctrl Pts',(-0.138911255368966,-1.,-2.04995762001328));
#29881=CARTESIAN_POINT('Ctrl Pts',(-0.138911255368966,1.,-2.04995762001328));
#29882=CARTESIAN_POINT('Ctrl Pts',(-0.140997332152546,-1.,-2.04414757947916));
#29883=CARTESIAN_POINT('Ctrl Pts',(-0.140997332152546,1.,-2.04414757947916));
#29884=CARTESIAN_POINT('Ctrl Pts',(-0.143035515058209,-1.,-2.03832911025912));
#29885=CARTESIAN_POINT('Ctrl Pts',(-0.143035515058209,1.,-2.03832911025912));
#29886=CARTESIAN_POINT('Ctrl Pts',(-0.145025140186057,-1.,-2.03250223739942));
#29887=CARTESIAN_POINT('Ctrl Pts',(-0.145025140186057,1.,-2.03250223739942));
#29888=CARTESIAN_POINT('Ctrl Pts',(-0.146965557332583,-1.,-2.02666926182017));
#29889=CARTESIAN_POINT('Ctrl Pts',(-0.146965557332583,1.,-2.02666926182017));
#29890=CARTESIAN_POINT('Ctrl Pts',(-0.148856124775337,-1.,-2.02083464969894));
#29891=CARTESIAN_POINT('Ctrl Pts',(-0.148856124775337,1.,-2.02083464969894));
#29892=CARTESIAN_POINT('Ctrl Pts',(-0.150696157673078,-1.,-2.01500291940238));
#29893=CARTESIAN_POINT('Ctrl Pts',(-0.150696157673078,1.,-2.01500291940238));
#29894=CARTESIAN_POINT('Ctrl Pts',(-0.15248488362145,-1.,-2.00917680318424));
#29895=CARTESIAN_POINT('Ctrl Pts',(-0.15248488362145,1.,-2.00917680318424));
#29896=CARTESIAN_POINT('Ctrl Pts',(-0.154221403049722,-1.,-2.00335565310543));
#29897=CARTESIAN_POINT('Ctrl Pts',(-0.154221403049722,1.,-2.00335565310543));
#29898=CARTESIAN_POINT('Ctrl Pts',(-0.155904629548783,-1.,-1.99753284771497));
#29899=CARTESIAN_POINT('Ctrl Pts',(-0.155904629548783,1.,-1.99753284771497));
#29900=CARTESIAN_POINT('Ctrl Pts',(-0.157533331459227,-1.,-1.99169810931908));
#29901=CARTESIAN_POINT('Ctrl Pts',(-0.157533331459227,1.,-1.99169810931908));
#29902=CARTESIAN_POINT('Ctrl Pts',(-0.159106226437299,-1.,-1.98584238283292));
#29903=CARTESIAN_POINT('Ctrl Pts',(-0.159106226437299,1.,-1.98584238283292));
#29904=CARTESIAN_POINT('Ctrl Pts',(-0.160622060784611,-1.,-1.97996195437559));
#29905=CARTESIAN_POINT('Ctrl Pts',(-0.160622060784611,1.,-1.97996195437559));
#29906=CARTESIAN_POINT('Ctrl Pts',(-0.162079693556289,-1.,-1.97406280235188));
#29907=CARTESIAN_POINT('Ctrl Pts',(-0.162079693556289,1.,-1.97406280235188));
#29908=CARTESIAN_POINT('Ctrl Pts',(-0.163478185457734,-1.,-1.96816512677967));
#29909=CARTESIAN_POINT('Ctrl Pts',(-0.163478185457734,1.,-1.96816512677967));
#29910=CARTESIAN_POINT('Ctrl Pts',(-0.164816568920269,-1.,-1.96229379940136));
#29911=CARTESIAN_POINT('Ctrl Pts',(-0.164816568920269,1.,-1.96229379940136));
#29912=CARTESIAN_POINT('Ctrl Pts',(-0.166093592002812,-1.,-1.9564675971873));
#29913=CARTESIAN_POINT('Ctrl Pts',(-0.166093592002812,1.,-1.9564675971873));
#29914=CARTESIAN_POINT('Ctrl Pts',(-0.167307501784475,-1.,-1.95069027794294));
#29915=CARTESIAN_POINT('Ctrl Pts',(-0.167307501784475,1.,-1.95069027794294));
#29916=CARTESIAN_POINT('Ctrl Pts',(-0.168455741607556,-1.,-1.94493757756931));
#29917=CARTESIAN_POINT('Ctrl Pts',(-0.168455741607556,1.,-1.94493757756931));
#29918=CARTESIAN_POINT('Ctrl Pts',(-0.169534904817491,-1.,-1.93915639211581));
#29919=CARTESIAN_POINT('Ctrl Pts',(-0.169534904817491,1.,-1.93915639211581));
#29920=CARTESIAN_POINT('Ctrl Pts',(-0.170541253116202,-1.,-1.93329183155539));
#29921=CARTESIAN_POINT('Ctrl Pts',(-0.170541253116202,1.,-1.93329183155539));
#29922=CARTESIAN_POINT('Ctrl Pts',(-0.171471191532988,-1.,-1.92731093582036));
#29923=CARTESIAN_POINT('Ctrl Pts',(-0.171471191532988,1.,-1.92731093582036));
#29924=CARTESIAN_POINT('Ctrl Pts',(-0.172321621259514,-1.,-1.9212233439798));
#29925=CARTESIAN_POINT('Ctrl Pts',(-0.172321621259514,1.,-1.9212233439798));
#29926=CARTESIAN_POINT('Ctrl Pts',(-0.173090695383496,-1.,-1.91511429159527));
#29927=CARTESIAN_POINT('Ctrl Pts',(-0.173090695383496,1.,-1.91511429159527));
#29928=CARTESIAN_POINT('Ctrl Pts',(-0.173776635257817,-1.,-1.90911693975267));
#29929=CARTESIAN_POINT('Ctrl Pts',(-0.173776635257817,1.,-1.90911693975267));
#29930=CARTESIAN_POINT('Ctrl Pts',(-0.174375518661085,-1.,-1.90335253862834));
#29931=CARTESIAN_POINT('Ctrl Pts',(-0.174375518661085,1.,-1.90335253862834));
#29932=CARTESIAN_POINT('Ctrl Pts',(-0.174879405091263,-1.,-1.89788101117132));
#29933=CARTESIAN_POINT('Ctrl Pts',(-0.174879405091263,1.,-1.89788101117132));
#29934=CARTESIAN_POINT('Ctrl Pts',(-0.175274276190844,-1.,-1.892646301985));
#29935=CARTESIAN_POINT('Ctrl Pts',(-0.175274276190844,1.,-1.892646301985));
#29936=CARTESIAN_POINT('Ctrl Pts',(-0.175538155840648,-1.,-1.88742606273259));
#29937=CARTESIAN_POINT('Ctrl Pts',(-0.175538155840648,1.,-1.88742606273259));
#29938=CARTESIAN_POINT('Ctrl Pts',(-0.175644148889699,-1.,-1.88188663145367));
#29939=CARTESIAN_POINT('Ctrl Pts',(-0.175644148889699,1.,-1.88188663145367));
#29940=CARTESIAN_POINT('Ctrl Pts',(-0.175563480746485,-1.,-1.87563767773588));
#29941=CARTESIAN_POINT('Ctrl Pts',(-0.175563480746485,1.,-1.87563767773588));
#29942=CARTESIAN_POINT('Ctrl Pts',(-0.175268337590758,-1.,-1.86828349694799));
#29943=CARTESIAN_POINT('Ctrl Pts',(-0.175268337590758,1.,-1.86828349694799));
#29944=CARTESIAN_POINT('Ctrl Pts',(-0.17473525927603,-1.,-1.85948367088837));
#29945=CARTESIAN_POINT('Ctrl Pts',(-0.17473525927603,1.,-1.85948367088837));
#29946=CARTESIAN_POINT('Ctrl Pts',(-0.173946627587731,-1.,-1.8489811319852));
#29947=CARTESIAN_POINT('Ctrl Pts',(-0.173946627587731,1.,-1.8489811319852));
#29948=CARTESIAN_POINT('Ctrl Pts',(-0.1728894428919,-1.,-1.83658380527692));
#29949=CARTESIAN_POINT('Ctrl Pts',(-0.1728894428919,1.,-1.83658380527692));
#29950=CARTESIAN_POINT('Ctrl Pts',(-0.171554770204119,-1.,-1.82215766811545));
#29951=CARTESIAN_POINT('Ctrl Pts',(-0.171554770204119,1.,-1.82215766811545));
#29952=CARTESIAN_POINT('Ctrl Pts',(-0.169936923904608,-1.,-1.80561530629706));
#29953=CARTESIAN_POINT('Ctrl Pts',(-0.169936923904608,1.,-1.80561530629706));
#29954=CARTESIAN_POINT('Ctrl Pts',(-0.168032772805197,-1.,-1.7869064998507));
#29955=CARTESIAN_POINT('Ctrl Pts',(-0.168032772805197,1.,-1.7869064998507));
#29956=CARTESIAN_POINT('Ctrl Pts',(-0.1662793551464,-1.,-1.77018771684844));
#29957=CARTESIAN_POINT('Ctrl Pts',(-0.1662793551464,1.,-1.77018771684844));
#29958=CARTESIAN_POINT('Ctrl Pts',(-0.164834765707158,-1.,-1.75666056638427));
#29959=CARTESIAN_POINT('Ctrl Pts',(-0.164834765707158,1.,-1.75666056638427));
#29960=CARTESIAN_POINT('Ctrl Pts',(-0.163814161002002,-1.,-1.7472034950333));
#29961=CARTESIAN_POINT('Ctrl Pts',(-0.163814161002002,1.,-1.7472034950333));
#29962=CARTESIAN_POINT('Ctrl Pts',(-0.163289472382896,-1.,-1.74236521665491));
#29963=CARTESIAN_POINT('Ctrl Pts',(-0.163289472382896,1.,-1.74236521665491));
#29964=CARTESIAN_POINT('',(-0.0694764450219581,1.,-2.19890268624765));
#29965=CARTESIAN_POINT('Ctrl Pts',(-0.0694764450219581,1.,-2.19890268624765));
#29966=CARTESIAN_POINT('Ctrl Pts',(-0.070114353632549,1.,-2.19777582085423));
#29967=CARTESIAN_POINT('Ctrl Pts',(-0.0713863779526154,1.,-2.19552129484002));
#29968=CARTESIAN_POINT('Ctrl Pts',(-0.0732830357306725,1.,-2.19213712013662));
#29969=CARTESIAN_POINT('Ctrl Pts',(-0.0757891465836148,1.,-2.1876201139953));
#29970=CARTESIAN_POINT('Ctrl Pts',(-0.0788837727685243,1.,-2.18196589448887));
#29971=CARTESIAN_POINT('Ctrl Pts',(-0.0819402680872765,1.,-2.176303712113));
#29972=CARTESIAN_POINT('Ctrl Pts',(-0.0849584620835372,1.,-2.17063357870952));
#29973=CARTESIAN_POINT('Ctrl Pts',(-0.0879381291386923,1.,-2.16495552645014));
#29974=CARTESIAN_POINT('Ctrl Pts',(-0.0908789888107265,1.,-2.15926961544516));
#29975=CARTESIAN_POINT('Ctrl Pts',(-0.0937807218867643,1.,-2.1535759397817));
#29976=CARTESIAN_POINT('Ctrl Pts',(-0.0966429852305459,1.,-2.14787463531795));
#29977=CARTESIAN_POINT('Ctrl Pts',(-0.0994654261990915,1.,-2.14216588396025));
#29978=CARTESIAN_POINT('Ctrl Pts',(-0.1022477005561,1.,-2.13644992667165));
#29979=CARTESIAN_POINT('Ctrl Pts',(-0.104989479152739,1.,-2.13072704887293));
#29980=CARTESIAN_POINT('Ctrl Pts',(-0.10769043523109,1.,-2.12499752307));
#29981=CARTESIAN_POINT('Ctrl Pts',(-0.110350236135025,1.,-2.11926155590865));
#29982=CARTESIAN_POINT('Ctrl Pts',(-0.112968534419737,1.,-2.11351924490306));
#29983=CARTESIAN_POINT('Ctrl Pts',(-0.115544957687926,1.,-2.10777050261309));
#29984=CARTESIAN_POINT('Ctrl Pts',(-0.118079107988355,1.,-2.102015121329));
#29985=CARTESIAN_POINT('Ctrl Pts',(-0.120570567965122,1.,-2.0962529286773));
#29986=CARTESIAN_POINT('Ctrl Pts',(-0.123018905621083,1.,-2.09048392424825));
#29987=CARTESIAN_POINT('Ctrl Pts',(-0.125423679412061,1.,-2.08470840653643));
#29988=CARTESIAN_POINT('Ctrl Pts',(-0.12778444527612,1.,-2.07892715110987));
#29989=CARTESIAN_POINT('Ctrl Pts',(-0.130100748328403,1.,-2.07314114713063));
#29990=CARTESIAN_POINT('Ctrl Pts',(-0.13237211154771,1.,-2.06735123910326));
#29991=CARTESIAN_POINT('Ctrl Pts',(-0.134598026192106,1.,-2.06155781517842));
#29992=CARTESIAN_POINT('Ctrl Pts',(-0.136777941218044,1.,-2.05576044414264));
#29993=CARTESIAN_POINT('Ctrl Pts',(-0.138911255368966,1.,-2.04995762001328));
#29994=CARTESIAN_POINT('Ctrl Pts',(-0.140997332152546,1.,-2.04414757947916));
#29995=CARTESIAN_POINT('Ctrl Pts',(-0.143035515058209,1.,-2.03832911025912));
#29996=CARTESIAN_POINT('Ctrl Pts',(-0.145025140186057,1.,-2.03250223739942));
#29997=CARTESIAN_POINT('Ctrl Pts',(-0.146965557332583,1.,-2.02666926182017));
#29998=CARTESIAN_POINT('Ctrl Pts',(-0.148856124775337,1.,-2.02083464969894));
#29999=CARTESIAN_POINT('Ctrl Pts',(-0.150696157673078,1.,-2.01500291940238));
#30000=CARTESIAN_POINT('Ctrl Pts',(-0.15248488362145,1.,-2.00917680318424));
#30001=CARTESIAN_POINT('Ctrl Pts',(-0.154221403049722,1.,-2.00335565310543));
#30002=CARTESIAN_POINT('Ctrl Pts',(-0.155904629548783,1.,-1.99753284771497));
#30003=CARTESIAN_POINT('Ctrl Pts',(-0.157533331459227,1.,-1.99169810931908));
#30004=CARTESIAN_POINT('Ctrl Pts',(-0.159106226437299,1.,-1.98584238283292));
#30005=CARTESIAN_POINT('Ctrl Pts',(-0.160622060784611,1.,-1.97996195437559));
#30006=CARTESIAN_POINT('Ctrl Pts',(-0.162079693556289,1.,-1.97406280235188));
#30007=CARTESIAN_POINT('Ctrl Pts',(-0.163478185457734,1.,-1.96816512677967));
#30008=CARTESIAN_POINT('Ctrl Pts',(-0.164816568920269,1.,-1.96229379940136));
#30009=CARTESIAN_POINT('Ctrl Pts',(-0.166093592002812,1.,-1.9564675971873));
#30010=CARTESIAN_POINT('Ctrl Pts',(-0.167307501784475,1.,-1.95069027794294));
#30011=CARTESIAN_POINT('Ctrl Pts',(-0.168455741607556,1.,-1.94493757756931));
#30012=CARTESIAN_POINT('Ctrl Pts',(-0.169534904817491,1.,-1.93915639211581));
#30013=CARTESIAN_POINT('Ctrl Pts',(-0.170541253116202,1.,-1.93329183155539));
#30014=CARTESIAN_POINT('Ctrl Pts',(-0.171471191532988,1.,-1.92731093582036));
#30015=CARTESIAN_POINT('Ctrl Pts',(-0.172321621259514,1.,-1.9212233439798));
#30016=CARTESIAN_POINT('Ctrl Pts',(-0.173090695383496,1.,-1.91511429159527));
#30017=CARTESIAN_POINT('Ctrl Pts',(-0.173776635257817,1.,-1.90911693975267));
#30018=CARTESIAN_POINT('Ctrl Pts',(-0.174375518661085,1.,-1.90335253862834));
#30019=CARTESIAN_POINT('Ctrl Pts',(-0.174879405091263,1.,-1.89788101117132));
#30020=CARTESIAN_POINT('Ctrl Pts',(-0.175274276190844,1.,-1.892646301985));
#30021=CARTESIAN_POINT('Ctrl Pts',(-0.175538155840648,1.,-1.88742606273259));
#30022=CARTESIAN_POINT('Ctrl Pts',(-0.175644148889699,1.,-1.88188663145367));
#30023=CARTESIAN_POINT('Ctrl Pts',(-0.175563480746485,1.,-1.87563767773588));
#30024=CARTESIAN_POINT('Ctrl Pts',(-0.175268337590758,1.,-1.86828349694799));
#30025=CARTESIAN_POINT('Ctrl Pts',(-0.17473525927603,1.,-1.85948367088837));
#30026=CARTESIAN_POINT('Ctrl Pts',(-0.173946627587731,1.,-1.8489811319852));
#30027=CARTESIAN_POINT('Ctrl Pts',(-0.1728894428919,1.,-1.83658380527692));
#30028=CARTESIAN_POINT('Ctrl Pts',(-0.171554770204119,1.,-1.82215766811545));
#30029=CARTESIAN_POINT('Ctrl Pts',(-0.169936923904608,1.,-1.80561530629706));
#30030=CARTESIAN_POINT('Ctrl Pts',(-0.168032772805197,1.,-1.7869064998507));
#30031=CARTESIAN_POINT('Ctrl Pts',(-0.1662793551464,1.,-1.77018771684844));
#30032=CARTESIAN_POINT('Ctrl Pts',(-0.164834765707158,1.,-1.75666056638427));
#30033=CARTESIAN_POINT('Ctrl Pts',(-0.163814161002002,1.,-1.7472034950333));
#30034=CARTESIAN_POINT('Ctrl Pts',(-0.163289472382896,1.,-1.74236521665491));
#30035=CARTESIAN_POINT('',(-0.0694764450219581,0.,-2.19890268624765));
#30036=CARTESIAN_POINT('Origin',(0.0694764450219584,0.,-2.19890268624765));
#30037=CARTESIAN_POINT('',(0.0694764450219584,1.,-2.19890268624765));
#30038=CARTESIAN_POINT('',(-0.0694764450219581,1.,-2.19890268624765));
#30039=CARTESIAN_POINT('',(0.0694764450219584,0.,-2.19890268624765));
#30040=CARTESIAN_POINT('Ctrl Pts',(0.163289472382896,-1.,-1.74236521665491));
#30041=CARTESIAN_POINT('Ctrl Pts',(0.163289472382896,1.,-1.74236521665491));
#30042=CARTESIAN_POINT('Ctrl Pts',(0.163814161002474,-1.,-1.74720349503904));
#30043=CARTESIAN_POINT('Ctrl Pts',(0.163814161002474,1.,-1.74720349503904));
#30044=CARTESIAN_POINT('Ctrl Pts',(0.164834765708484,-1.,-1.75666056640041));
#30045=CARTESIAN_POINT('Ctrl Pts',(0.164834765708484,1.,-1.75666056640041));
#30046=CARTESIAN_POINT('Ctrl Pts',(0.166279355148738,-1.,-1.77018771687692));
#30047=CARTESIAN_POINT('Ctrl Pts',(0.166279355148738,1.,-1.77018771687692));
#30048=CARTESIAN_POINT('Ctrl Pts',(0.16803277280837,-1.,-1.78690649988931));
#30049=CARTESIAN_POINT('Ctrl Pts',(0.16803277280837,1.,-1.78690649988931));
#30050=CARTESIAN_POINT('Ctrl Pts',(0.169936923908078,-1.,-1.80561530633924));
#30051=CARTESIAN_POINT('Ctrl Pts',(0.169936923908078,1.,-1.80561530633924));
#30052=CARTESIAN_POINT('Ctrl Pts',(0.171554770207306,-1.,-1.82215766815414));
#30053=CARTESIAN_POINT('Ctrl Pts',(0.171554770207306,1.,-1.82215766815414));
#30054=CARTESIAN_POINT('Ctrl Pts',(0.17288944289442,-1.,-1.83658380530747));
#30055=CARTESIAN_POINT('Ctrl Pts',(0.17288944289442,1.,-1.83658380530747));
#30056=CARTESIAN_POINT('Ctrl Pts',(0.173946627589401,-1.,-1.84898113200543));
#30057=CARTESIAN_POINT('Ctrl Pts',(0.173946627589401,1.,-1.84898113200543));
#30058=CARTESIAN_POINT('Ctrl Pts',(0.174735259276856,-1.,-1.85948367089838));
#30059=CARTESIAN_POINT('Ctrl Pts',(0.174735259276856,1.,-1.85948367089838));
#30060=CARTESIAN_POINT('Ctrl Pts',(0.175268337590901,-1.,-1.86828349694972));
#30061=CARTESIAN_POINT('Ctrl Pts',(0.175268337590901,1.,-1.86828349694972));
#30062=CARTESIAN_POINT('Ctrl Pts',(0.175563480746205,-1.,-1.87563767773249));
#30063=CARTESIAN_POINT('Ctrl Pts',(0.175563480746205,1.,-1.87563767773249));
#30064=CARTESIAN_POINT('Ctrl Pts',(0.175644148889271,-1.,-1.88188663144846));
#30065=CARTESIAN_POINT('Ctrl Pts',(0.175644148889271,1.,-1.88188663144846));
#30066=CARTESIAN_POINT('Ctrl Pts',(0.175538155840286,-1.,-1.88742606272818));
#30067=CARTESIAN_POINT('Ctrl Pts',(0.175538155840286,1.,-1.88742606272818));
#30068=CARTESIAN_POINT('Ctrl Pts',(0.175274276190664,-1.,-1.89264630198279));
#30069=CARTESIAN_POINT('Ctrl Pts',(0.175274276190664,1.,-1.89264630198279));
#30070=CARTESIAN_POINT('Ctrl Pts',(0.174879405091277,-1.,-1.89788101117148));
#30071=CARTESIAN_POINT('Ctrl Pts',(0.174879405091277,1.,-1.89788101117148));
#30072=CARTESIAN_POINT('Ctrl Pts',(0.174375518661222,-1.,-1.90335253863003));
#30073=CARTESIAN_POINT('Ctrl Pts',(0.174375518661222,1.,-1.90335253863003));
#30074=CARTESIAN_POINT('Ctrl Pts',(0.173776635257984,-1.,-1.90911693975475));
#30075=CARTESIAN_POINT('Ctrl Pts',(0.173776635257984,1.,-1.90911693975475));
#30076=CARTESIAN_POINT('Ctrl Pts',(0.173090695383619,-1.,-1.91511429159681));
#30077=CARTESIAN_POINT('Ctrl Pts',(0.173090695383619,1.,-1.91511429159681));
#30078=CARTESIAN_POINT('Ctrl Pts',(0.172321621259557,-1.,-1.92122334398034));
#30079=CARTESIAN_POINT('Ctrl Pts',(0.172321621259557,1.,-1.92122334398034));
#30080=CARTESIAN_POINT('Ctrl Pts',(0.17147119153296,-1.,-1.92731093582));
#30081=CARTESIAN_POINT('Ctrl Pts',(0.17147119153296,1.,-1.92731093582));
#30082=CARTESIAN_POINT('Ctrl Pts',(0.170541253116136,-1.,-1.93329183155455));
#30083=CARTESIAN_POINT('Ctrl Pts',(0.170541253116136,1.,-1.93329183155455));
#30084=CARTESIAN_POINT('Ctrl Pts',(0.169534904817425,-1.,-1.93915639211497));
#30085=CARTESIAN_POINT('Ctrl Pts',(0.169534904817425,1.,-1.93915639211497));
#30086=CARTESIAN_POINT('Ctrl Pts',(0.168455741607516,-1.,-1.94493757756879));
#30087=CARTESIAN_POINT('Ctrl Pts',(0.168455741607516,1.,-1.94493757756879));
#30088=CARTESIAN_POINT('Ctrl Pts',(0.167307501784469,-1.,-1.95069027794286));
#30089=CARTESIAN_POINT('Ctrl Pts',(0.167307501784469,1.,-1.95069027794286));
#30090=CARTESIAN_POINT('Ctrl Pts',(0.166093592002833,-1.,-1.95646759718755));
#30091=CARTESIAN_POINT('Ctrl Pts',(0.166093592002833,1.,-1.95646759718755));
#30092=CARTESIAN_POINT('Ctrl Pts',(0.1648165689203,-1.,-1.96229379940174));
#30093=CARTESIAN_POINT('Ctrl Pts',(0.1648165689203,1.,-1.96229379940174));
#30094=CARTESIAN_POINT('Ctrl Pts',(0.16347818545776,-1.,-1.96816512678));
#30095=CARTESIAN_POINT('Ctrl Pts',(0.16347818545776,1.,-1.96816512678));
#30096=CARTESIAN_POINT('Ctrl Pts',(0.162079693556302,-1.,-1.97406280235204));
#30097=CARTESIAN_POINT('Ctrl Pts',(0.162079693556302,1.,-1.97406280235204));
#30098=CARTESIAN_POINT('Ctrl Pts',(0.16062206078461,-1.,-1.97996195437557));
#30099=CARTESIAN_POINT('Ctrl Pts',(0.16062206078461,1.,-1.97996195437557));
#30100=CARTESIAN_POINT('Ctrl Pts',(0.159106226437288,-1.,-1.98584238283279));
#30101=CARTESIAN_POINT('Ctrl Pts',(0.159106226437288,1.,-1.98584238283279));
#30102=CARTESIAN_POINT('Ctrl Pts',(0.157533331459215,-1.,-1.99169810931893));
#30103=CARTESIAN_POINT('Ctrl Pts',(0.157533331459215,1.,-1.99169810931893));
#30104=CARTESIAN_POINT('Ctrl Pts',(0.155904629548774,-1.,-1.99753284771487));
#30105=CARTESIAN_POINT('Ctrl Pts',(0.155904629548774,1.,-1.99753284771487));
#30106=CARTESIAN_POINT('Ctrl Pts',(0.154221403049719,-1.,-2.00335565310539));
#30107=CARTESIAN_POINT('Ctrl Pts',(0.154221403049719,1.,-2.00335565310539));
#30108=CARTESIAN_POINT('Ctrl Pts',(0.152484883621452,-1.,-2.00917680318426));
#30109=CARTESIAN_POINT('Ctrl Pts',(0.152484883621452,1.,-2.00917680318426));
#30110=CARTESIAN_POINT('Ctrl Pts',(0.150696157673084,-1.,-2.01500291940243));
#30111=CARTESIAN_POINT('Ctrl Pts',(0.150696157673084,1.,-2.01500291940243));
#30112=CARTESIAN_POINT('Ctrl Pts',(0.148856124775343,-1.,-2.02083464969897));
#30113=CARTESIAN_POINT('Ctrl Pts',(0.148856124775343,1.,-2.02083464969897));
#30114=CARTESIAN_POINT('Ctrl Pts',(0.146965557332586,-1.,-2.02666926182017));
#30115=CARTESIAN_POINT('Ctrl Pts',(0.146965557332586,1.,-2.02666926182017));
#30116=CARTESIAN_POINT('Ctrl Pts',(0.145025140186058,-1.,-2.03250223739941));
#30117=CARTESIAN_POINT('Ctrl Pts',(0.145025140186058,1.,-2.03250223739941));
#30118=CARTESIAN_POINT('Ctrl Pts',(0.143035515058208,-1.,-2.03832911025913));
#30119=CARTESIAN_POINT('Ctrl Pts',(0.143035515058208,1.,-2.03832911025913));
#30120=CARTESIAN_POINT('Ctrl Pts',(0.140997332152545,-1.,-2.04414757947919));
#30121=CARTESIAN_POINT('Ctrl Pts',(0.140997332152545,1.,-2.04414757947919));
#30122=CARTESIAN_POINT('Ctrl Pts',(0.138911255368966,-1.,-2.04995762001333));
#30123=CARTESIAN_POINT('Ctrl Pts',(0.138911255368966,1.,-2.04995762001333));
#30124=CARTESIAN_POINT('Ctrl Pts',(0.136777941218044,-1.,-2.0557604441427));
#30125=CARTESIAN_POINT('Ctrl Pts',(0.136777941218044,1.,-2.0557604441427));
#30126=CARTESIAN_POINT('Ctrl Pts',(0.134598026192107,-1.,-2.06155781517844));
#30127=CARTESIAN_POINT('Ctrl Pts',(0.134598026192107,1.,-2.06155781517844));
#30128=CARTESIAN_POINT('Ctrl Pts',(0.13237211154771,-1.,-2.06735123910319));
#30129=CARTESIAN_POINT('Ctrl Pts',(0.13237211154771,1.,-2.06735123910319));
#30130=CARTESIAN_POINT('Ctrl Pts',(0.1301007483284,-1.,-2.07314114713047));
#30131=CARTESIAN_POINT('Ctrl Pts',(0.1301007483284,1.,-2.07314114713047));
#30132=CARTESIAN_POINT('Ctrl Pts',(0.127784445276116,-1.,-2.07892715110967));
#30133=CARTESIAN_POINT('Ctrl Pts',(0.127784445276116,1.,-2.07892715110967));
#30134=CARTESIAN_POINT('Ctrl Pts',(0.125423679412058,-1.,-2.08470840653628));
#30135=CARTESIAN_POINT('Ctrl Pts',(0.125423679412058,1.,-2.08470840653628));
#30136=CARTESIAN_POINT('Ctrl Pts',(0.123018905621083,-1.,-2.09048392424826));
#30137=CARTESIAN_POINT('Ctrl Pts',(0.123018905621083,1.,-2.09048392424826));
#30138=CARTESIAN_POINT('Ctrl Pts',(0.120570567965129,-1.,-2.09625292867756));
#30139=CARTESIAN_POINT('Ctrl Pts',(0.120570567965129,1.,-2.09625292867756));
#30140=CARTESIAN_POINT('Ctrl Pts',(0.118079107988368,-1.,-2.10201512132945));
#30141=CARTESIAN_POINT('Ctrl Pts',(0.118079107988368,1.,-2.10201512132945));
#30142=CARTESIAN_POINT('Ctrl Pts',(0.11554495768794,-1.,-2.10777050261359));
#30143=CARTESIAN_POINT('Ctrl Pts',(0.11554495768794,1.,-2.10777050261359));
#30144=CARTESIAN_POINT('Ctrl Pts',(0.112968534419746,-1.,-2.11351924490335));
#30145=CARTESIAN_POINT('Ctrl Pts',(0.112968534419746,1.,-2.11351924490335));
#30146=CARTESIAN_POINT('Ctrl Pts',(0.11035023613502,-1.,-2.11926155590849));
#30147=CARTESIAN_POINT('Ctrl Pts',(0.11035023613502,1.,-2.11926155590849));
#30148=CARTESIAN_POINT('Ctrl Pts',(0.107690435231068,-1.,-2.12499752306927));
#30149=CARTESIAN_POINT('Ctrl Pts',(0.107690435231068,1.,-2.12499752306927));
#30150=CARTESIAN_POINT('Ctrl Pts',(0.104989479152703,-1.,-2.1307270488718));
#30151=CARTESIAN_POINT('Ctrl Pts',(0.104989479152703,1.,-2.1307270488718));
#30152=CARTESIAN_POINT('Ctrl Pts',(0.102247700556064,-1.,-2.13644992667052));
#30153=CARTESIAN_POINT('Ctrl Pts',(0.102247700556064,1.,-2.13644992667052));
#30154=CARTESIAN_POINT('Ctrl Pts',(0.0994654261990743,-1.,-2.14216588395974));
#30155=CARTESIAN_POINT('Ctrl Pts',(0.0994654261990743,1.,-2.14216588395974));
#30156=CARTESIAN_POINT('Ctrl Pts',(0.0966429852305689,-1.,-2.14787463531864));
#30157=CARTESIAN_POINT('Ctrl Pts',(0.0966429852305689,1.,-2.14787463531864));
#30158=CARTESIAN_POINT('Ctrl Pts',(0.0937807218868345,-1.,-2.15357593978377));
#30159=CARTESIAN_POINT('Ctrl Pts',(0.0937807218868345,1.,-2.15357593978377));
#30160=CARTESIAN_POINT('Ctrl Pts',(0.0908789888108266,-1.,-2.15926961544808));
#30161=CARTESIAN_POINT('Ctrl Pts',(0.0908789888108266,1.,-2.15926961544808));
#30162=CARTESIAN_POINT('Ctrl Pts',(0.0879381291387823,-1.,-2.16495552645275));
#30163=CARTESIAN_POINT('Ctrl Pts',(0.0879381291387823,1.,-2.16495552645275));
#30164=CARTESIAN_POINT('Ctrl Pts',(0.0849584620835643,-1.,-2.17063357871031));
#30165=CARTESIAN_POINT('Ctrl Pts',(0.0849584620835643,1.,-2.17063357871031));
#30166=CARTESIAN_POINT('Ctrl Pts',(0.0819402680871939,-1.,-2.1763037121106));
#30167=CARTESIAN_POINT('Ctrl Pts',(0.0819402680871939,1.,-2.1763037121106));
#30168=CARTESIAN_POINT('Ctrl Pts',(0.0788837727683228,-1.,-2.18196589448304));
#30169=CARTESIAN_POINT('Ctrl Pts',(0.0788837727683228,1.,-2.18196589448304));
#30170=CARTESIAN_POINT('Ctrl Pts',(0.0757891465833411,-1.,-2.1876201139874));
#30171=CARTESIAN_POINT('Ctrl Pts',(0.0757891465833411,1.,-2.1876201139874));
#30172=CARTESIAN_POINT('Ctrl Pts',(0.0732830357304276,-1.,-2.19213712012956));
#30173=CARTESIAN_POINT('Ctrl Pts',(0.0732830357304276,1.,-2.19213712012956));
#30174=CARTESIAN_POINT('Ctrl Pts',(0.0713863779524627,-1.,-2.19552129483562));
#30175=CARTESIAN_POINT('Ctrl Pts',(0.0713863779524627,1.,-2.19552129483562));
#30176=CARTESIAN_POINT('Ctrl Pts',(0.0701143536324926,-1.,-2.19777582085261));
#30177=CARTESIAN_POINT('Ctrl Pts',(0.0701143536324926,1.,-2.19777582085261));
#30178=CARTESIAN_POINT('Ctrl Pts',(0.0694764450219584,-1.,-2.19890268624765));
#30179=CARTESIAN_POINT('Ctrl Pts',(0.0694764450219584,1.,-2.19890268624765));
#30180=CARTESIAN_POINT('',(0.163289472382896,1.,-1.74236521665491));
#30181=CARTESIAN_POINT('Ctrl Pts',(0.163289472382896,1.,-1.74236521665491));
#30182=CARTESIAN_POINT('Ctrl Pts',(0.163814161002474,1.,-1.74720349503904));
#30183=CARTESIAN_POINT('Ctrl Pts',(0.164834765708484,1.,-1.75666056640041));
#30184=CARTESIAN_POINT('Ctrl Pts',(0.166279355148738,1.,-1.77018771687692));
#30185=CARTESIAN_POINT('Ctrl Pts',(0.16803277280837,1.,-1.78690649988931));
#30186=CARTESIAN_POINT('Ctrl Pts',(0.169936923908078,1.,-1.80561530633924));
#30187=CARTESIAN_POINT('Ctrl Pts',(0.171554770207306,1.,-1.82215766815414));
#30188=CARTESIAN_POINT('Ctrl Pts',(0.17288944289442,1.,-1.83658380530747));
#30189=CARTESIAN_POINT('Ctrl Pts',(0.173946627589401,1.,-1.84898113200543));
#30190=CARTESIAN_POINT('Ctrl Pts',(0.174735259276856,1.,-1.85948367089838));
#30191=CARTESIAN_POINT('Ctrl Pts',(0.175268337590901,1.,-1.86828349694972));
#30192=CARTESIAN_POINT('Ctrl Pts',(0.175563480746205,1.,-1.87563767773249));
#30193=CARTESIAN_POINT('Ctrl Pts',(0.175644148889271,1.,-1.88188663144846));
#30194=CARTESIAN_POINT('Ctrl Pts',(0.175538155840286,1.,-1.88742606272818));
#30195=CARTESIAN_POINT('Ctrl Pts',(0.175274276190664,1.,-1.89264630198279));
#30196=CARTESIAN_POINT('Ctrl Pts',(0.174879405091277,1.,-1.89788101117148));
#30197=CARTESIAN_POINT('Ctrl Pts',(0.174375518661222,1.,-1.90335253863003));
#30198=CARTESIAN_POINT('Ctrl Pts',(0.173776635257984,1.,-1.90911693975475));
#30199=CARTESIAN_POINT('Ctrl Pts',(0.173090695383619,1.,-1.91511429159681));
#30200=CARTESIAN_POINT('Ctrl Pts',(0.172321621259557,1.,-1.92122334398034));
#30201=CARTESIAN_POINT('Ctrl Pts',(0.17147119153296,1.,-1.92731093582));
#30202=CARTESIAN_POINT('Ctrl Pts',(0.170541253116136,1.,-1.93329183155455));
#30203=CARTESIAN_POINT('Ctrl Pts',(0.169534904817425,1.,-1.93915639211497));
#30204=CARTESIAN_POINT('Ctrl Pts',(0.168455741607516,1.,-1.94493757756879));
#30205=CARTESIAN_POINT('Ctrl Pts',(0.167307501784469,1.,-1.95069027794286));
#30206=CARTESIAN_POINT('Ctrl Pts',(0.166093592002833,1.,-1.95646759718755));
#30207=CARTESIAN_POINT('Ctrl Pts',(0.1648165689203,1.,-1.96229379940174));
#30208=CARTESIAN_POINT('Ctrl Pts',(0.16347818545776,1.,-1.96816512678));
#30209=CARTESIAN_POINT('Ctrl Pts',(0.162079693556302,1.,-1.97406280235204));
#30210=CARTESIAN_POINT('Ctrl Pts',(0.16062206078461,1.,-1.97996195437557));
#30211=CARTESIAN_POINT('Ctrl Pts',(0.159106226437288,1.,-1.98584238283279));
#30212=CARTESIAN_POINT('Ctrl Pts',(0.157533331459215,1.,-1.99169810931893));
#30213=CARTESIAN_POINT('Ctrl Pts',(0.155904629548774,1.,-1.99753284771487));
#30214=CARTESIAN_POINT('Ctrl Pts',(0.154221403049719,1.,-2.00335565310539));
#30215=CARTESIAN_POINT('Ctrl Pts',(0.152484883621452,1.,-2.00917680318426));
#30216=CARTESIAN_POINT('Ctrl Pts',(0.150696157673084,1.,-2.01500291940243));
#30217=CARTESIAN_POINT('Ctrl Pts',(0.148856124775343,1.,-2.02083464969897));
#30218=CARTESIAN_POINT('Ctrl Pts',(0.146965557332586,1.,-2.02666926182017));
#30219=CARTESIAN_POINT('Ctrl Pts',(0.145025140186058,1.,-2.03250223739941));
#30220=CARTESIAN_POINT('Ctrl Pts',(0.143035515058208,1.,-2.03832911025913));
#30221=CARTESIAN_POINT('Ctrl Pts',(0.140997332152545,1.,-2.04414757947919));
#30222=CARTESIAN_POINT('Ctrl Pts',(0.138911255368966,1.,-2.04995762001333));
#30223=CARTESIAN_POINT('Ctrl Pts',(0.136777941218044,1.,-2.0557604441427));
#30224=CARTESIAN_POINT('Ctrl Pts',(0.134598026192107,1.,-2.06155781517844));
#30225=CARTESIAN_POINT('Ctrl Pts',(0.13237211154771,1.,-2.06735123910319));
#30226=CARTESIAN_POINT('Ctrl Pts',(0.1301007483284,1.,-2.07314114713047));
#30227=CARTESIAN_POINT('Ctrl Pts',(0.127784445276116,1.,-2.07892715110967));
#30228=CARTESIAN_POINT('Ctrl Pts',(0.125423679412058,1.,-2.08470840653628));
#30229=CARTESIAN_POINT('Ctrl Pts',(0.123018905621083,1.,-2.09048392424826));
#30230=CARTESIAN_POINT('Ctrl Pts',(0.120570567965129,1.,-2.09625292867756));
#30231=CARTESIAN_POINT('Ctrl Pts',(0.118079107988368,1.,-2.10201512132945));
#30232=CARTESIAN_POINT('Ctrl Pts',(0.11554495768794,1.,-2.10777050261359));
#30233=CARTESIAN_POINT('Ctrl Pts',(0.112968534419746,1.,-2.11351924490335));
#30234=CARTESIAN_POINT('Ctrl Pts',(0.11035023613502,1.,-2.11926155590849));
#30235=CARTESIAN_POINT('Ctrl Pts',(0.107690435231068,1.,-2.12499752306927));
#30236=CARTESIAN_POINT('Ctrl Pts',(0.104989479152703,1.,-2.1307270488718));
#30237=CARTESIAN_POINT('Ctrl Pts',(0.102247700556064,1.,-2.13644992667052));
#30238=CARTESIAN_POINT('Ctrl Pts',(0.0994654261990743,1.,-2.14216588395974));
#30239=CARTESIAN_POINT('Ctrl Pts',(0.0966429852305689,1.,-2.14787463531864));
#30240=CARTESIAN_POINT('Ctrl Pts',(0.0937807218868345,1.,-2.15357593978377));
#30241=CARTESIAN_POINT('Ctrl Pts',(0.0908789888108266,1.,-2.15926961544808));
#30242=CARTESIAN_POINT('Ctrl Pts',(0.0879381291387823,1.,-2.16495552645275));
#30243=CARTESIAN_POINT('Ctrl Pts',(0.0849584620835643,1.,-2.17063357871031));
#30244=CARTESIAN_POINT('Ctrl Pts',(0.0819402680871939,1.,-2.1763037121106));
#30245=CARTESIAN_POINT('Ctrl Pts',(0.0788837727683228,1.,-2.18196589448304));
#30246=CARTESIAN_POINT('Ctrl Pts',(0.0757891465833411,1.,-2.1876201139874));
#30247=CARTESIAN_POINT('Ctrl Pts',(0.0732830357304276,1.,-2.19213712012956));
#30248=CARTESIAN_POINT('Ctrl Pts',(0.0713863779524627,1.,-2.19552129483562));
#30249=CARTESIAN_POINT('Ctrl Pts',(0.0701143536324926,1.,-2.19777582085261));
#30250=CARTESIAN_POINT('Ctrl Pts',(0.0694764450219584,1.,-2.19890268624765));
#30251=CARTESIAN_POINT('',(0.163289472382896,0.,-1.74236521665491));
#30252=CARTESIAN_POINT('Origin',(0.,0.,0.));
#30253=CARTESIAN_POINT('',(0.383122945602004,1.,-1.7075470150345));
#30254=CARTESIAN_POINT('Origin',(0.,1.,0.));
#30255=CARTESIAN_POINT('',(0.383122945602004,0.,-1.7075470150345));
#30256=CARTESIAN_POINT('Ctrl Pts',(0.61342227326009,-1.,-2.11275013067528));
#30257=CARTESIAN_POINT('Ctrl Pts',(0.61342227326009,1.,-2.11275013067528));
#30258=CARTESIAN_POINT('Ctrl Pts',(0.61246736556225,-1.,-2.11187554260142));
#30259=CARTESIAN_POINT('Ctrl Pts',(0.61246736556225,1.,-2.11187554260142));
#30260=CARTESIAN_POINT('Ctrl Pts',(0.610560911691113,-1.,-2.11012443807661));
#30261=CARTESIAN_POINT('Ctrl Pts',(0.610560911691113,1.,-2.11012443807661));
#30262=CARTESIAN_POINT('Ctrl Pts',(0.607711315456826,-1.,-2.10749199615859));
#30263=CARTESIAN_POINT('Ctrl Pts',(0.607711315456826,1.,-2.10749199615859));
#30264=CARTESIAN_POINT('Ctrl Pts',(0.603932030738212,-1.,-2.10397049887709));
#30265=CARTESIAN_POINT('Ctrl Pts',(0.603932030738212,1.,-2.10397049887709));
#30266=CARTESIAN_POINT('Ctrl Pts',(0.599241616422144,-1.,-2.09954930865331));
#30267=CARTESIAN_POINT('Ctrl Pts',(0.599241616422144,1.,-2.09954930865331));
#30268=CARTESIAN_POINT('Ctrl Pts',(0.594585006052823,-1.,-2.09510876220501));
#30269=CARTESIAN_POINT('Ctrl Pts',(0.594585006052823,1.,-2.09510876220501));
#30270=CARTESIAN_POINT('Ctrl Pts',(0.589962365403189,-1.,-2.09064881812053));
#30271=CARTESIAN_POINT('Ctrl Pts',(0.589962365403189,1.,-2.09064881812053));
#30272=CARTESIAN_POINT('Ctrl Pts',(0.585373918990895,-1.,-2.086169437277));
#30273=CARTESIAN_POINT('Ctrl Pts',(0.585373918990895,1.,-2.086169437277));
#30274=CARTESIAN_POINT('Ctrl Pts',(0.580819952107256,-1.,-2.08167059018138));
#30275=CARTESIAN_POINT('Ctrl Pts',(0.580819952107256,1.,-2.08167059018138));
#30276=CARTESIAN_POINT('Ctrl Pts',(0.576300797416274,-1.,-2.07715226767361));
#30277=CARTESIAN_POINT('Ctrl Pts',(0.576300797416274,1.,-2.07715226767361));
#30278=CARTESIAN_POINT('Ctrl Pts',(0.571816823242411,-1.,-2.07261449292758));
#30279=CARTESIAN_POINT('Ctrl Pts',(0.571816823242411,1.,-2.07261449292758));
#30280=CARTESIAN_POINT('Ctrl Pts',(0.567368421181229,-1.,-2.06805732997383));
#30281=CARTESIAN_POINT('Ctrl Pts',(0.567368421181229,1.,-2.06805732997383));
#30282=CARTESIAN_POINT('Ctrl Pts',(0.562955993082574,-1.,-2.06348090160697));
#30283=CARTESIAN_POINT('Ctrl Pts',(0.562955993082574,1.,-2.06348090160697));
#30284=CARTESIAN_POINT('Ctrl Pts',(0.558579940185467,-1.,-2.05888537756571));
#30285=CARTESIAN_POINT('Ctrl Pts',(0.558579940185467,1.,-2.05888537756571));
#30286=CARTESIAN_POINT('Ctrl Pts',(0.554240657464109,-1.,-2.05427091604482));
#30287=CARTESIAN_POINT('Ctrl Pts',(0.554240657464109,1.,-2.05427091604482));
#30288=CARTESIAN_POINT('Ctrl Pts',(0.549938525150342,-1.,-2.04963761077974));
#30289=CARTESIAN_POINT('Ctrl Pts',(0.549938525150342,1.,-2.04963761077974));
#30290=CARTESIAN_POINT('Ctrl Pts',(0.545673903817348,-1.,-2.0449854471456));
#30291=CARTESIAN_POINT('Ctrl Pts',(0.545673903817348,1.,-2.0449854471456));
#30292=CARTESIAN_POINT('Ctrl Pts',(0.54144712061552,-1.,-2.0403142269048));
#30293=CARTESIAN_POINT('Ctrl Pts',(0.54144712061552,1.,-2.0403142269048));
#30294=CARTESIAN_POINT('Ctrl Pts',(0.537258489833134,-1.,-2.03562362953993));
#30295=CARTESIAN_POINT('Ctrl Pts',(0.537258489833134,1.,-2.03562362953993));
#30296=CARTESIAN_POINT('Ctrl Pts',(0.533108355132905,-1.,-2.03091336214401));
#30297=CARTESIAN_POINT('Ctrl Pts',(0.533108355132905,1.,-2.03091336214401));
#30298=CARTESIAN_POINT('Ctrl Pts',(0.52899712724191,-1.,-2.02618329083289));
#30299=CARTESIAN_POINT('Ctrl Pts',(0.52899712724191,1.,-2.02618329083289));
#30300=CARTESIAN_POINT('Ctrl Pts',(0.524925318333518,-1.,-2.02143356304712));
#30301=CARTESIAN_POINT('Ctrl Pts',(0.524925318333518,1.,-2.02143356304712));
#30302=CARTESIAN_POINT('Ctrl Pts',(0.520893590399428,-1.,-2.01666477917306));
#30303=CARTESIAN_POINT('Ctrl Pts',(0.520893590399428,1.,-2.01666477917306));
#30304=CARTESIAN_POINT('Ctrl Pts',(0.516902681728733,-1.,-2.01187773939257));
#30305=CARTESIAN_POINT('Ctrl Pts',(0.516902681728733,1.,-2.01187773939257));
#30306=CARTESIAN_POINT('Ctrl Pts',(0.512953306961813,-1.,-2.00707309946955));
#30307=CARTESIAN_POINT('Ctrl Pts',(0.512953306961813,1.,-2.00707309946955));
#30308=CARTESIAN_POINT('Ctrl Pts',(0.509046069886152,-1.,-2.00225107134733));
#30309=CARTESIAN_POINT('Ctrl Pts',(0.509046069886152,1.,-2.00225107134733));
#30310=CARTESIAN_POINT('Ctrl Pts',(0.505181361323011,-1.,-1.99741107463567));
#30311=CARTESIAN_POINT('Ctrl Pts',(0.505181361323011,1.,-1.99741107463567));
#30312=CARTESIAN_POINT('Ctrl Pts',(0.501359287727129,-1.,-1.9925514912615));
#30313=CARTESIAN_POINT('Ctrl Pts',(0.501359287727129,1.,-1.9925514912615));
#30314=CARTESIAN_POINT('Ctrl Pts',(0.497579909545564,-1.,-1.98767044752929));
#30315=CARTESIAN_POINT('Ctrl Pts',(0.497579909545564,1.,-1.98767044752929));
#30316=CARTESIAN_POINT('Ctrl Pts',(0.493843476541492,-1.,-1.9827665876182));
#30317=CARTESIAN_POINT('Ctrl Pts',(0.493843476541492,1.,-1.9827665876182));
#30318=CARTESIAN_POINT('Ctrl Pts',(0.490150627860955,-1.,-1.97783973019229));
#30319=CARTESIAN_POINT('Ctrl Pts',(0.490150627860955,1.,-1.97783973019229));
#30320=CARTESIAN_POINT('Ctrl Pts',(0.486502692907661,-1.,-1.97289186263272));
#30321=CARTESIAN_POINT('Ctrl Pts',(0.486502692907661,1.,-1.97289186263272));
#30322=CARTESIAN_POINT('Ctrl Pts',(0.482901662120686,-1.,-1.96792703422358));
#30323=CARTESIAN_POINT('Ctrl Pts',(0.482901662120686,1.,-1.96792703422358));
#30324=CARTESIAN_POINT('Ctrl Pts',(0.479349583074846,-1.,-1.96294933055938));
#30325=CARTESIAN_POINT('Ctrl Pts',(0.479349583074846,1.,-1.96294933055938));
#30326=CARTESIAN_POINT('Ctrl Pts',(0.475848034683171,-1.,-1.95796111148175));
#30327=CARTESIAN_POINT('Ctrl Pts',(0.475848034683171,1.,-1.95796111148175));
#30328=CARTESIAN_POINT('Ctrl Pts',(0.472397672264079,-1.,-1.95296148278136));
#30329=CARTESIAN_POINT('Ctrl Pts',(0.472397672264079,1.,-1.95296148278136));
#30330=CARTESIAN_POINT('Ctrl Pts',(0.468997482913158,-1.,-1.94794381136524));
#30331=CARTESIAN_POINT('Ctrl Pts',(0.468997482913158,1.,-1.94794381136524));
#30332=CARTESIAN_POINT('Ctrl Pts',(0.465645462026064,-1.,-1.94289794196205));
#30333=CARTESIAN_POINT('Ctrl Pts',(0.465645462026064,1.,-1.94289794196205));
#30334=CARTESIAN_POINT('Ctrl Pts',(0.462340031009087,-1.,-1.93781486640834));
#30335=CARTESIAN_POINT('Ctrl Pts',(0.462340031009087,1.,-1.93781486640834));
#30336=CARTESIAN_POINT('Ctrl Pts',(0.459081234547931,-1.,-1.93269066517936));
#30337=CARTESIAN_POINT('Ctrl Pts',(0.459081234547931,1.,-1.93269066517936));
#30338=CARTESIAN_POINT('Ctrl Pts',(0.455872005174335,-1.,-1.92753067150461));
#30339=CARTESIAN_POINT('Ctrl Pts',(0.455872005174335,1.,-1.92753067150461));
#30340=CARTESIAN_POINT('Ctrl Pts',(0.452719478359356,-1.,-1.9223538064847));
#30341=CARTESIAN_POINT('Ctrl Pts',(0.452719478359356,1.,-1.9223538064847));
#30342=CARTESIAN_POINT('Ctrl Pts',(0.449632260106572,-1.,-1.91718342555717));
#30343=CARTESIAN_POINT('Ctrl Pts',(0.449632260106572,1.,-1.91718342555717));
#30344=CARTESIAN_POINT('Ctrl Pts',(0.446617343485651,-1.,-1.91203699981095));
#30345=CARTESIAN_POINT('Ctrl Pts',(0.446617343485651,1.,-1.91203699981095));
#30346=CARTESIAN_POINT('Ctrl Pts',(0.44367755684917,-1.,-1.90691756144906));
#30347=CARTESIAN_POINT('Ctrl Pts',(0.44367755684917,1.,-1.90691756144906));
#30348=CARTESIAN_POINT('Ctrl Pts',(0.44080783370416,-1.,-1.90180124389137));
#30349=CARTESIAN_POINT('Ctrl Pts',(0.44080783370416,1.,-1.90180124389137));
#30350=CARTESIAN_POINT('Ctrl Pts',(0.437995003948443,-1.,-1.89663648956549));
#30351=CARTESIAN_POINT('Ctrl Pts',(0.437995003948443,1.,-1.89663648956549));
#30352=CARTESIAN_POINT('Ctrl Pts',(0.43522566096358,-1.,-1.89136993975585));
#30353=CARTESIAN_POINT('Ctrl Pts',(0.43522566096358,1.,-1.89136993975585));
#30354=CARTESIAN_POINT('Ctrl Pts',(0.432493038548833,-1.,-1.88596913666828));
#30355=CARTESIAN_POINT('Ctrl Pts',(0.432493038548833,1.,-1.88596913666828));
#30356=CARTESIAN_POINT('Ctrl Pts',(0.429803062482217,-1.,-1.88044229001779));
#30357=CARTESIAN_POINT('Ctrl Pts',(0.429803062482217,1.,-1.88044229001779));
#30358=CARTESIAN_POINT('Ctrl Pts',(0.427183828518743,-1.,-1.87486989291334));
#30359=CARTESIAN_POINT('Ctrl Pts',(0.427183828518743,1.,-1.87486989291334));
#30360=CARTESIAN_POINT('Ctrl Pts',(0.424678177290876,-1.,-1.8693780394412));
#30361=CARTESIAN_POINT('Ctrl Pts',(0.424678177290876,1.,-1.8693780394412));
#30362=CARTESIAN_POINT('Ctrl Pts',(0.422327307417884,-1.,-1.86408083333863));
#30363=CARTESIAN_POINT('Ctrl Pts',(0.422327307417884,1.,-1.86408083333863));
#30364=CARTESIAN_POINT('Ctrl Pts',(0.420157287975583,-1.,-1.8590328109667));
#30365=CARTESIAN_POINT('Ctrl Pts',(0.420157287975583,1.,-1.8590328109667));
#30366=CARTESIAN_POINT('Ctrl Pts',(0.418164129144045,-1.,-1.8541763285645));
#30367=CARTESIAN_POINT('Ctrl Pts',(0.418164129144045,1.,-1.8541763285645));
#30368=CARTESIAN_POINT('Ctrl Pts',(0.416300022039885,-1.,-1.84929312930314));
#30369=CARTESIAN_POINT('Ctrl Pts',(0.416300022039885,1.,-1.84929312930314));
#30370=CARTESIAN_POINT('Ctrl Pts',(0.414487438255542,-1.,-1.84405757074218));
#30371=CARTESIAN_POINT('Ctrl Pts',(0.414487438255542,1.,-1.84405757074218));
#30372=CARTESIAN_POINT('Ctrl Pts',(0.412633125322945,-1.,-1.8380895347617));
#30373=CARTESIAN_POINT('Ctrl Pts',(0.412633125322945,1.,-1.8380895347617));
#30374=CARTESIAN_POINT('Ctrl Pts',(0.410641256301276,-1.,-1.83100408895047));
#30375=CARTESIAN_POINT('Ctrl Pts',(0.410641256301276,1.,-1.83100408895047));
#30376=CARTESIAN_POINT('Ctrl Pts',(0.408428948106227,-1.,-1.82247022677562));
#30377=CARTESIAN_POINT('Ctrl Pts',(0.408428948106227,1.,-1.82247022677562));
#30378=CARTESIAN_POINT('Ctrl Pts',(0.405933518407175,-1.,-1.81223801812013));
#30379=CARTESIAN_POINT('Ctrl Pts',(0.405933518407175,1.,-1.81223801812013));
#30380=CARTESIAN_POINT('Ctrl Pts',(0.403107976163396,-1.,-1.80012077173238));
#30381=CARTESIAN_POINT('Ctrl Pts',(0.403107976163396,1.,-1.80012077173238));
#30382=CARTESIAN_POINT('Ctrl Pts',(0.399919403774155,-1.,-1.78598826343754));
#30383=CARTESIAN_POINT('Ctrl Pts',(0.399919403774155,1.,-1.78598826343754));
#30384=CARTESIAN_POINT('Ctrl Pts',(0.396346196110688,-1.,-1.76975560043442));
#30385=CARTESIAN_POINT('Ctrl Pts',(0.396346196110688,1.,-1.76975560043442));
#30386=CARTESIAN_POINT('Ctrl Pts',(0.392375812285395,-1.,-1.75137405310193));
#30387=CARTESIAN_POINT('Ctrl Pts',(0.392375812285395,1.,-1.75137405310193));
#30388=CARTESIAN_POINT('Ctrl Pts',(0.388877023502615,-1.,-1.73493170972829));
#30389=CARTESIAN_POINT('Ctrl Pts',(0.388877023502615,1.,-1.73493170972829));
#30390=CARTESIAN_POINT('Ctrl Pts',(0.386070790323281,-1.,-1.72162022244582));
#30391=CARTESIAN_POINT('Ctrl Pts',(0.386070790323281,1.,-1.72162022244582));
#30392=CARTESIAN_POINT('Ctrl Pts',(0.384119047314215,-1.,-1.71231062891398));
#30393=CARTESIAN_POINT('Ctrl Pts',(0.384119047314215,1.,-1.71231062891398));
#30394=CARTESIAN_POINT('Ctrl Pts',(0.383122945602004,-1.,-1.7075470150345));
#30395=CARTESIAN_POINT('Ctrl Pts',(0.383122945602004,1.,-1.7075470150345));
#30396=CARTESIAN_POINT('',(0.61342227326009,1.,-2.11275013067528));
#30397=CARTESIAN_POINT('Ctrl Pts',(0.61342227326009,1.,-2.11275013067528));
#30398=CARTESIAN_POINT('Ctrl Pts',(0.61246736556225,1.,-2.11187554260142));
#30399=CARTESIAN_POINT('Ctrl Pts',(0.610560911691113,1.,-2.11012443807661));
#30400=CARTESIAN_POINT('Ctrl Pts',(0.607711315456826,1.,-2.10749199615859));
#30401=CARTESIAN_POINT('Ctrl Pts',(0.603932030738212,1.,-2.10397049887709));
#30402=CARTESIAN_POINT('Ctrl Pts',(0.599241616422144,1.,-2.09954930865331));
#30403=CARTESIAN_POINT('Ctrl Pts',(0.594585006052823,1.,-2.09510876220501));
#30404=CARTESIAN_POINT('Ctrl Pts',(0.589962365403189,1.,-2.09064881812053));
#30405=CARTESIAN_POINT('Ctrl Pts',(0.585373918990895,1.,-2.086169437277));
#30406=CARTESIAN_POINT('Ctrl Pts',(0.580819952107256,1.,-2.08167059018138));
#30407=CARTESIAN_POINT('Ctrl Pts',(0.576300797416274,1.,-2.07715226767361));
#30408=CARTESIAN_POINT('Ctrl Pts',(0.571816823242411,1.,-2.07261449292758));
#30409=CARTESIAN_POINT('Ctrl Pts',(0.567368421181229,1.,-2.06805732997383));
#30410=CARTESIAN_POINT('Ctrl Pts',(0.562955993082574,1.,-2.06348090160697));
#30411=CARTESIAN_POINT('Ctrl Pts',(0.558579940185467,1.,-2.05888537756571));
#30412=CARTESIAN_POINT('Ctrl Pts',(0.554240657464109,1.,-2.05427091604482));
#30413=CARTESIAN_POINT('Ctrl Pts',(0.549938525150342,1.,-2.04963761077974));
#30414=CARTESIAN_POINT('Ctrl Pts',(0.545673903817348,1.,-2.0449854471456));
#30415=CARTESIAN_POINT('Ctrl Pts',(0.54144712061552,1.,-2.0403142269048));
#30416=CARTESIAN_POINT('Ctrl Pts',(0.537258489833134,1.,-2.03562362953993));
#30417=CARTESIAN_POINT('Ctrl Pts',(0.533108355132905,1.,-2.03091336214401));
#30418=CARTESIAN_POINT('Ctrl Pts',(0.52899712724191,1.,-2.02618329083289));
#30419=CARTESIAN_POINT('Ctrl Pts',(0.524925318333518,1.,-2.02143356304712));
#30420=CARTESIAN_POINT('Ctrl Pts',(0.520893590399428,1.,-2.01666477917306));
#30421=CARTESIAN_POINT('Ctrl Pts',(0.516902681728733,1.,-2.01187773939257));
#30422=CARTESIAN_POINT('Ctrl Pts',(0.512953306961813,1.,-2.00707309946955));
#30423=CARTESIAN_POINT('Ctrl Pts',(0.509046069886152,1.,-2.00225107134733));
#30424=CARTESIAN_POINT('Ctrl Pts',(0.505181361323011,1.,-1.99741107463567));
#30425=CARTESIAN_POINT('Ctrl Pts',(0.501359287727129,1.,-1.9925514912615));
#30426=CARTESIAN_POINT('Ctrl Pts',(0.497579909545564,1.,-1.98767044752929));
#30427=CARTESIAN_POINT('Ctrl Pts',(0.493843476541492,1.,-1.9827665876182));
#30428=CARTESIAN_POINT('Ctrl Pts',(0.490150627860955,1.,-1.97783973019229));
#30429=CARTESIAN_POINT('Ctrl Pts',(0.486502692907661,1.,-1.97289186263272));
#30430=CARTESIAN_POINT('Ctrl Pts',(0.482901662120686,1.,-1.96792703422358));
#30431=CARTESIAN_POINT('Ctrl Pts',(0.479349583074846,1.,-1.96294933055938));
#30432=CARTESIAN_POINT('Ctrl Pts',(0.475848034683171,1.,-1.95796111148175));
#30433=CARTESIAN_POINT('Ctrl Pts',(0.472397672264079,1.,-1.95296148278136));
#30434=CARTESIAN_POINT('Ctrl Pts',(0.468997482913158,1.,-1.94794381136524));
#30435=CARTESIAN_POINT('Ctrl Pts',(0.465645462026064,1.,-1.94289794196205));
#30436=CARTESIAN_POINT('Ctrl Pts',(0.462340031009087,1.,-1.93781486640834));
#30437=CARTESIAN_POINT('Ctrl Pts',(0.459081234547931,1.,-1.93269066517936));
#30438=CARTESIAN_POINT('Ctrl Pts',(0.455872005174335,1.,-1.92753067150461));
#30439=CARTESIAN_POINT('Ctrl Pts',(0.452719478359356,1.,-1.9223538064847));
#30440=CARTESIAN_POINT('Ctrl Pts',(0.449632260106572,1.,-1.91718342555717));
#30441=CARTESIAN_POINT('Ctrl Pts',(0.446617343485651,1.,-1.91203699981095));
#30442=CARTESIAN_POINT('Ctrl Pts',(0.44367755684917,1.,-1.90691756144906));
#30443=CARTESIAN_POINT('Ctrl Pts',(0.44080783370416,1.,-1.90180124389137));
#30444=CARTESIAN_POINT('Ctrl Pts',(0.437995003948443,1.,-1.89663648956549));
#30445=CARTESIAN_POINT('Ctrl Pts',(0.43522566096358,1.,-1.89136993975585));
#30446=CARTESIAN_POINT('Ctrl Pts',(0.432493038548833,1.,-1.88596913666828));
#30447=CARTESIAN_POINT('Ctrl Pts',(0.429803062482217,1.,-1.88044229001779));
#30448=CARTESIAN_POINT('Ctrl Pts',(0.427183828518743,1.,-1.87486989291334));
#30449=CARTESIAN_POINT('Ctrl Pts',(0.424678177290876,1.,-1.8693780394412));
#30450=CARTESIAN_POINT('Ctrl Pts',(0.422327307417884,1.,-1.86408083333863));
#30451=CARTESIAN_POINT('Ctrl Pts',(0.420157287975583,1.,-1.8590328109667));
#30452=CARTESIAN_POINT('Ctrl Pts',(0.418164129144045,1.,-1.8541763285645));
#30453=CARTESIAN_POINT('Ctrl Pts',(0.416300022039885,1.,-1.84929312930314));
#30454=CARTESIAN_POINT('Ctrl Pts',(0.414487438255542,1.,-1.84405757074218));
#30455=CARTESIAN_POINT('Ctrl Pts',(0.412633125322945,1.,-1.8380895347617));
#30456=CARTESIAN_POINT('Ctrl Pts',(0.410641256301276,1.,-1.83100408895047));
#30457=CARTESIAN_POINT('Ctrl Pts',(0.408428948106227,1.,-1.82247022677562));
#30458=CARTESIAN_POINT('Ctrl Pts',(0.405933518407175,1.,-1.81223801812013));
#30459=CARTESIAN_POINT('Ctrl Pts',(0.403107976163396,1.,-1.80012077173238));
#30460=CARTESIAN_POINT('Ctrl Pts',(0.399919403774155,1.,-1.78598826343754));
#30461=CARTESIAN_POINT('Ctrl Pts',(0.396346196110688,1.,-1.76975560043442));
#30462=CARTESIAN_POINT('Ctrl Pts',(0.392375812285395,1.,-1.75137405310193));
#30463=CARTESIAN_POINT('Ctrl Pts',(0.388877023502615,1.,-1.73493170972829));
#30464=CARTESIAN_POINT('Ctrl Pts',(0.386070790323281,1.,-1.72162022244582));
#30465=CARTESIAN_POINT('Ctrl Pts',(0.384119047314215,1.,-1.71231062891398));
#30466=CARTESIAN_POINT('Ctrl Pts',(0.383122945602004,1.,-1.7075470150345));
#30467=CARTESIAN_POINT('',(0.61342227326009,0.,-2.11275013067528));
#30468=CARTESIAN_POINT('Origin',(0.745574324794401,0.,-2.0698113262342));
#30469=CARTESIAN_POINT('',(0.745574324794401,1.,-2.0698113262342));
#30470=CARTESIAN_POINT('',(0.61342227326009,1.,-2.11275013067528));
#30471=CARTESIAN_POINT('',(0.745574324794401,0.,-2.0698113262342));
#30472=CARTESIAN_POINT('Ctrl Pts',(0.693717979106306,-1.,-1.60662857109684));
#30473=CARTESIAN_POINT('Ctrl Pts',(0.693717979106306,1.,-1.60662857109684));
#30474=CARTESIAN_POINT('Ctrl Pts',(0.695712097881194,-1.,-1.61106790958151));
#30475=CARTESIAN_POINT('Ctrl Pts',(0.695712097881194,1.,-1.61106790958151));
#30476=CARTESIAN_POINT('Ctrl Pts',(0.699605146405088,-1.,-1.61974673472612));
#30477=CARTESIAN_POINT('Ctrl Pts',(0.699605146405088,1.,-1.61974673472612));
#30478=CARTESIAN_POINT('Ctrl Pts',(0.705159151988319,-1.,-1.63216541664676));
#30479=CARTESIAN_POINT('Ctrl Pts',(0.705159151988319,1.,-1.63216541664676));
#30480=CARTESIAN_POINT('Ctrl Pts',(0.711993139355394,-1.,-1.64752408832016));
#30481=CARTESIAN_POINT('Ctrl Pts',(0.711993139355394,1.,-1.64752408832016));
#30482=CARTESIAN_POINT('Ctrl Pts',(0.719585433804282,-1.,-1.6647288055568));
#30483=CARTESIAN_POINT('Ctrl Pts',(0.719585433804282,1.,-1.6647288055568));
#30484=CARTESIAN_POINT('Ctrl Pts',(0.726235967997433,-1.,-1.67996158455503));
#30485=CARTESIAN_POINT('Ctrl Pts',(0.726235967997433,1.,-1.67996158455503));
#30486=CARTESIAN_POINT('Ctrl Pts',(0.731963238697195,-1.,-1.69326921975743));
#30487=CARTESIAN_POINT('Ctrl Pts',(0.731963238697195,1.,-1.69326921975743));
#30488=CARTESIAN_POINT('Ctrl Pts',(0.736799665724771,-1.,-1.70473309006121));
#30489=CARTESIAN_POINT('Ctrl Pts',(0.736799665724771,1.,-1.70473309006121));
#30490=CARTESIAN_POINT('Ctrl Pts',(0.740795162032087,-1.,-1.71447789751927));
#30491=CARTESIAN_POINT('Ctrl Pts',(0.740795162032087,1.,-1.71447789751927));
#30492=CARTESIAN_POINT('Ctrl Pts',(0.744021445433764,-1.,-1.7226822991693));
#30493=CARTESIAN_POINT('Ctrl Pts',(0.744021445433764,1.,-1.7226822991693));
#30494=CARTESIAN_POINT('Ctrl Pts',(0.746574710096436,-1.,-1.72958533647399));
#30495=CARTESIAN_POINT('Ctrl Pts',(0.746574710096436,1.,-1.72958533647399));
#30496=CARTESIAN_POINT('Ctrl Pts',(0.748582462954854,-1.,-1.73550351679848));
#30497=CARTESIAN_POINT('Ctrl Pts',(0.748582462954854,1.,-1.73550351679848));
#30498=CARTESIAN_POINT('Ctrl Pts',(0.75019343597954,-1.,-1.74080458266705));
#30499=CARTESIAN_POINT('Ctrl Pts',(0.75019343597954,1.,-1.74080458266705));
#30500=CARTESIAN_POINT('Ctrl Pts',(0.751555614163629,-1.,-1.74585086852298));
#30501=CARTESIAN_POINT('Ctrl Pts',(0.751555614163629,1.,-1.74585086852298));
#30502=CARTESIAN_POINT('Ctrl Pts',(0.752797683531377,-1.,-1.75095139468809));
#30503=CARTESIAN_POINT('Ctrl Pts',(0.752797683531377,1.,-1.75095139468809));
#30504=CARTESIAN_POINT('Ctrl Pts',(0.75400925402848,-1.,-1.75631083600175));
#30505=CARTESIAN_POINT('Ctrl Pts',(0.75400925402848,1.,-1.75631083600175));
#30506=CARTESIAN_POINT('Ctrl Pts',(0.755220979975262,-1.,-1.7619781724032));
#30507=CARTESIAN_POINT('Ctrl Pts',(0.755220979975262,1.,-1.7619781724032));
#30508=CARTESIAN_POINT('Ctrl Pts',(0.756421896028403,-1.,-1.76789396003141));
#30509=CARTESIAN_POINT('Ctrl Pts',(0.756421896028403,1.,-1.76789396003141));
#30510=CARTESIAN_POINT('Ctrl Pts',(0.757578264077238,-1.,-1.77394167108342));
#30511=CARTESIAN_POINT('Ctrl Pts',(0.757578264077238,1.,-1.77394167108342));
#30512=CARTESIAN_POINT('Ctrl Pts',(0.75865062667738,-1.,-1.77999411220912));
#30513=CARTESIAN_POINT('Ctrl Pts',(0.75865062667738,1.,-1.77999411220912));
#30514=CARTESIAN_POINT('Ctrl Pts',(0.759614401109868,-1.,-1.78596964884527));
#30515=CARTESIAN_POINT('Ctrl Pts',(0.759614401109868,1.,-1.78596964884527));
#30516=CARTESIAN_POINT('Ctrl Pts',(0.760469555880425,-1.,-1.79185815610802));
#30517=CARTESIAN_POINT('Ctrl Pts',(0.760469555880425,1.,-1.79185815610802));
#30518=CARTESIAN_POINT('Ctrl Pts',(0.761229695230359,-1.,-1.79768986997735));
#30519=CARTESIAN_POINT('Ctrl Pts',(0.761229695230359,1.,-1.79768986997735));
#30520=CARTESIAN_POINT('Ctrl Pts',(0.761915336443515,-1.,-1.80351583877334));
#30521=CARTESIAN_POINT('Ctrl Pts',(0.761915336443515,1.,-1.80351583877334));
#30522=CARTESIAN_POINT('Ctrl Pts',(0.762546129464036,-1.,-1.80938551463989));
#30523=CARTESIAN_POINT('Ctrl Pts',(0.762546129464036,1.,-1.80938551463989));
#30524=CARTESIAN_POINT('Ctrl Pts',(0.763132003836783,-1.,-1.81532118405566));
#30525=CARTESIAN_POINT('Ctrl Pts',(0.763132003836783,1.,-1.81532118405566));
#30526=CARTESIAN_POINT('Ctrl Pts',(0.763673465462854,-1.,-1.82131873145297));
#30527=CARTESIAN_POINT('Ctrl Pts',(0.763673465462854,1.,-1.82131873145297));
#30528=CARTESIAN_POINT('Ctrl Pts',(0.764165902606055,-1.,-1.8273599120008));
#30529=CARTESIAN_POINT('Ctrl Pts',(0.764165902606055,1.,-1.8273599120008));
#30530=CARTESIAN_POINT('Ctrl Pts',(0.764602549687845,-1.,-1.8334207722714));
#30531=CARTESIAN_POINT('Ctrl Pts',(0.764602549687845,1.,-1.8334207722714));
#30532=CARTESIAN_POINT('Ctrl Pts',(0.764978057881687,-1.,-1.83948181064823));
#30533=CARTESIAN_POINT('Ctrl Pts',(0.764978057881687,1.,-1.83948181064823));
#30534=CARTESIAN_POINT('Ctrl Pts',(0.765291664861971,-1.,-1.84553698875911));
#30535=CARTESIAN_POINT('Ctrl Pts',(0.765291664861971,1.,-1.84553698875911));
#30536=CARTESIAN_POINT('Ctrl Pts',(0.765545710619023,-1.,-1.85158945130054));
#30537=CARTESIAN_POINT('Ctrl Pts',(0.765545710619023,1.,-1.85158945130054));
#30538=CARTESIAN_POINT('Ctrl Pts',(0.765744212909305,-1.,-1.85764741390391));
#30539=CARTESIAN_POINT('Ctrl Pts',(0.765744212909305,1.,-1.85764741390391));
#30540=CARTESIAN_POINT('Ctrl Pts',(0.765891519092557,-1.,-1.86372027063315));
#30541=CARTESIAN_POINT('Ctrl Pts',(0.765891519092557,1.,-1.86372027063315));
#30542=CARTESIAN_POINT('Ctrl Pts',(0.765990708546111,-1.,-1.86981398314345));
#30543=CARTESIAN_POINT('Ctrl Pts',(0.765990708546111,1.,-1.86981398314345));
#30544=CARTESIAN_POINT('Ctrl Pts',(0.766042837036759,-1.,-1.87592888967886));
#30545=CARTESIAN_POINT('Ctrl Pts',(0.766042837036759,1.,-1.87592888967886));
#30546=CARTESIAN_POINT('Ctrl Pts',(0.766047794851868,-1.,-1.88206215302561));
#30547=CARTESIAN_POINT('Ctrl Pts',(0.766047794851868,1.,-1.88206215302561));
#30548=CARTESIAN_POINT('Ctrl Pts',(0.76600483706209,-1.,-1.88820926433409));
#30549=CARTESIAN_POINT('Ctrl Pts',(0.76600483706209,1.,-1.88820926433409));
#30550=CARTESIAN_POINT('Ctrl Pts',(0.765913193856979,-1.,-1.89436577771389));
#30551=CARTESIAN_POINT('Ctrl Pts',(0.765913193856979,1.,-1.89436577771389));
#30552=CARTESIAN_POINT('Ctrl Pts',(0.765772772593395,-1.,-1.90052930393599));
#30553=CARTESIAN_POINT('Ctrl Pts',(0.765772772593395,1.,-1.90052930393599));
#30554=CARTESIAN_POINT('Ctrl Pts',(0.765584196937936,-1.,-1.90669961402362));
#30555=CARTESIAN_POINT('Ctrl Pts',(0.765584196937936,1.,-1.90669961402362));
#30556=CARTESIAN_POINT('Ctrl Pts',(0.765348465884739,-1.,-1.91287765805174));
#30557=CARTESIAN_POINT('Ctrl Pts',(0.765348465884739,1.,-1.91287765805174));
#30558=CARTESIAN_POINT('Ctrl Pts',(0.765066729667095,-1.,-1.91906491634197));
#30559=CARTESIAN_POINT('Ctrl Pts',(0.765066729667095,1.,-1.91906491634197));
#30560=CARTESIAN_POINT('Ctrl Pts',(0.764740025488189,-1.,-1.92526263537041));
#30561=CARTESIAN_POINT('Ctrl Pts',(0.764740025488189,1.,-1.92526263537041));
#30562=CARTESIAN_POINT('Ctrl Pts',(0.764369010673889,-1.,-1.93147105496367));
#30563=CARTESIAN_POINT('Ctrl Pts',(0.764369010673889,1.,-1.93147105496367));
#30564=CARTESIAN_POINT('Ctrl Pts',(0.763954049121393,-1.,-1.93768964875867));
#30565=CARTESIAN_POINT('Ctrl Pts',(0.763954049121393,1.,-1.93768964875867));
#30566=CARTESIAN_POINT('Ctrl Pts',(0.76349533353858,-1.,-1.94391746617626));
#30567=CARTESIAN_POINT('Ctrl Pts',(0.76349533353858,1.,-1.94391746617626));
#30568=CARTESIAN_POINT('Ctrl Pts',(0.762992990878774,-1.,-1.95015342590025));
#30569=CARTESIAN_POINT('Ctrl Pts',(0.762992990878774,1.,-1.95015342590025));
#30570=CARTESIAN_POINT('Ctrl Pts',(0.762447203806263,-1.,-1.95639665309893));
#30571=CARTESIAN_POINT('Ctrl Pts',(0.762447203806263,1.,-1.95639665309893));
#30572=CARTESIAN_POINT('Ctrl Pts',(0.761858300014575,-1.,-1.96264672744229));
#30573=CARTESIAN_POINT('Ctrl Pts',(0.761858300014575,1.,-1.96264672744229));
#30574=CARTESIAN_POINT('Ctrl Pts',(0.761226690483986,-1.,-1.96890351582545));
#30575=CARTESIAN_POINT('Ctrl Pts',(0.761226690483986,1.,-1.96890351582545));
#30576=CARTESIAN_POINT('Ctrl Pts',(0.760552825409855,-1.,-1.97516705321521));
#30577=CARTESIAN_POINT('Ctrl Pts',(0.760552825409855,1.,-1.97516705321521));
#30578=CARTESIAN_POINT('Ctrl Pts',(0.759837147452135,-1.,-1.98143741418156));
#30579=CARTESIAN_POINT('Ctrl Pts',(0.759837147452135,1.,-1.98143741418156));
#30580=CARTESIAN_POINT('Ctrl Pts',(0.759080037802242,-1.,-1.98771456680806));
#30581=CARTESIAN_POINT('Ctrl Pts',(0.759080037802242,1.,-1.98771456680806));
#30582=CARTESIAN_POINT('Ctrl Pts',(0.758281796766377,-1.,-1.9939983109871));
#30583=CARTESIAN_POINT('Ctrl Pts',(0.758281796766377,1.,-1.9939983109871));
#30584=CARTESIAN_POINT('Ctrl Pts',(0.757442676862341,-1.,-2.00028834739072));
#30585=CARTESIAN_POINT('Ctrl Pts',(0.757442676862341,1.,-2.00028834739072));
#30586=CARTESIAN_POINT('Ctrl Pts',(0.756562904646496,-1.,-2.00658431587682));
#30587=CARTESIAN_POINT('Ctrl Pts',(0.756562904646496,1.,-2.00658431587682));
#30588=CARTESIAN_POINT('Ctrl Pts',(0.7556427049581,-1.,-2.01288584328149));
#30589=CARTESIAN_POINT('Ctrl Pts',(0.7556427049581,1.,-2.01288584328149));
#30590=CARTESIAN_POINT('Ctrl Pts',(0.75468233072352,-1.,-2.01919259406003));
#30591=CARTESIAN_POINT('Ctrl Pts',(0.75468233072352,1.,-2.01919259406003));
#30592=CARTESIAN_POINT('Ctrl Pts',(0.753682061113765,-1.,-2.02550428623587));
#30593=CARTESIAN_POINT('Ctrl Pts',(0.753682061113765,1.,-2.02550428623587));
#30594=CARTESIAN_POINT('Ctrl Pts',(0.752642180488104,-1.,-2.03182068456467));
#30595=CARTESIAN_POINT('Ctrl Pts',(0.752642180488104,1.,-2.03182068456467));
#30596=CARTESIAN_POINT('Ctrl Pts',(0.751562963361383,-1.,-2.03814160092173));
#30597=CARTESIAN_POINT('Ctrl Pts',(0.751562963361383,1.,-2.03814160092173));
#30598=CARTESIAN_POINT('Ctrl Pts',(0.750444657874758,-1.,-2.04446689147754));
#30599=CARTESIAN_POINT('Ctrl Pts',(0.750444657874758,1.,-2.04446689147754));
#30600=CARTESIAN_POINT('Ctrl Pts',(0.749287468663053,-1.,-2.05079645591606));
#30601=CARTESIAN_POINT('Ctrl Pts',(0.749287468663053,1.,-2.05079645591606));
#30602=CARTESIAN_POINT('Ctrl Pts',(0.748091554181101,-1.,-2.05713023030263));
#30603=CARTESIAN_POINT('Ctrl Pts',(0.748091554181101,1.,-2.05713023030263));
#30604=CARTESIAN_POINT('Ctrl Pts',(0.747103932785504,-1.,-2.06220058927162));
#30605=CARTESIAN_POINT('Ctrl Pts',(0.747103932785504,1.,-2.06220058927162));
#30606=CARTESIAN_POINT('Ctrl Pts',(0.746345871542695,-1.,-2.06600523016401));
#30607=CARTESIAN_POINT('Ctrl Pts',(0.746345871542695,1.,-2.06600523016401));
#30608=CARTESIAN_POINT('Ctrl Pts',(0.74583279137781,-1.,-2.06854248895575));
#30609=CARTESIAN_POINT('Ctrl Pts',(0.74583279137781,1.,-2.06854248895575));
#30610=CARTESIAN_POINT('Ctrl Pts',(0.745574324794401,-1.,-2.0698113262342));
#30611=CARTESIAN_POINT('Ctrl Pts',(0.745574324794401,1.,-2.0698113262342));
#30612=CARTESIAN_POINT('',(0.693717979106306,1.,-1.60662857109684));
#30613=CARTESIAN_POINT('Ctrl Pts',(0.693717979106306,1.,-1.60662857109684));
#30614=CARTESIAN_POINT('Ctrl Pts',(0.695712097881194,1.,-1.61106790958151));
#30615=CARTESIAN_POINT('Ctrl Pts',(0.699605146405088,1.,-1.61974673472612));
#30616=CARTESIAN_POINT('Ctrl Pts',(0.705159151988319,1.,-1.63216541664676));
#30617=CARTESIAN_POINT('Ctrl Pts',(0.711993139355394,1.,-1.64752408832016));
#30618=CARTESIAN_POINT('Ctrl Pts',(0.719585433804282,1.,-1.6647288055568));
#30619=CARTESIAN_POINT('Ctrl Pts',(0.726235967997433,1.,-1.67996158455503));
#30620=CARTESIAN_POINT('Ctrl Pts',(0.731963238697195,1.,-1.69326921975743));
#30621=CARTESIAN_POINT('Ctrl Pts',(0.736799665724771,1.,-1.70473309006121));
#30622=CARTESIAN_POINT('Ctrl Pts',(0.740795162032087,1.,-1.71447789751927));
#30623=CARTESIAN_POINT('Ctrl Pts',(0.744021445433764,1.,-1.7226822991693));
#30624=CARTESIAN_POINT('Ctrl Pts',(0.746574710096436,1.,-1.72958533647399));
#30625=CARTESIAN_POINT('Ctrl Pts',(0.748582462954854,1.,-1.73550351679848));
#30626=CARTESIAN_POINT('Ctrl Pts',(0.75019343597954,1.,-1.74080458266705));
#30627=CARTESIAN_POINT('Ctrl Pts',(0.751555614163629,1.,-1.74585086852298));
#30628=CARTESIAN_POINT('Ctrl Pts',(0.752797683531377,1.,-1.75095139468809));
#30629=CARTESIAN_POINT('Ctrl Pts',(0.75400925402848,1.,-1.75631083600175));
#30630=CARTESIAN_POINT('Ctrl Pts',(0.755220979975262,1.,-1.7619781724032));
#30631=CARTESIAN_POINT('Ctrl Pts',(0.756421896028403,1.,-1.76789396003141));
#30632=CARTESIAN_POINT('Ctrl Pts',(0.757578264077238,1.,-1.77394167108342));
#30633=CARTESIAN_POINT('Ctrl Pts',(0.75865062667738,1.,-1.77999411220912));
#30634=CARTESIAN_POINT('Ctrl Pts',(0.759614401109868,1.,-1.78596964884527));
#30635=CARTESIAN_POINT('Ctrl Pts',(0.760469555880425,1.,-1.79185815610802));
#30636=CARTESIAN_POINT('Ctrl Pts',(0.761229695230359,1.,-1.79768986997735));
#30637=CARTESIAN_POINT('Ctrl Pts',(0.761915336443515,1.,-1.80351583877334));
#30638=CARTESIAN_POINT('Ctrl Pts',(0.762546129464036,1.,-1.80938551463989));
#30639=CARTESIAN_POINT('Ctrl Pts',(0.763132003836783,1.,-1.81532118405566));
#30640=CARTESIAN_POINT('Ctrl Pts',(0.763673465462854,1.,-1.82131873145297));
#30641=CARTESIAN_POINT('Ctrl Pts',(0.764165902606055,1.,-1.8273599120008));
#30642=CARTESIAN_POINT('Ctrl Pts',(0.764602549687845,1.,-1.8334207722714));
#30643=CARTESIAN_POINT('Ctrl Pts',(0.764978057881687,1.,-1.83948181064823));
#30644=CARTESIAN_POINT('Ctrl Pts',(0.765291664861971,1.,-1.84553698875911));
#30645=CARTESIAN_POINT('Ctrl Pts',(0.765545710619023,1.,-1.85158945130054));
#30646=CARTESIAN_POINT('Ctrl Pts',(0.765744212909305,1.,-1.85764741390391));
#30647=CARTESIAN_POINT('Ctrl Pts',(0.765891519092557,1.,-1.86372027063315));
#30648=CARTESIAN_POINT('Ctrl Pts',(0.765990708546111,1.,-1.86981398314345));
#30649=CARTESIAN_POINT('Ctrl Pts',(0.766042837036759,1.,-1.87592888967886));
#30650=CARTESIAN_POINT('Ctrl Pts',(0.766047794851868,1.,-1.88206215302561));
#30651=CARTESIAN_POINT('Ctrl Pts',(0.76600483706209,1.,-1.88820926433409));
#30652=CARTESIAN_POINT('Ctrl Pts',(0.765913193856979,1.,-1.89436577771389));
#30653=CARTESIAN_POINT('Ctrl Pts',(0.765772772593395,1.,-1.90052930393599));
#30654=CARTESIAN_POINT('Ctrl Pts',(0.765584196937936,1.,-1.90669961402362));
#30655=CARTESIAN_POINT('Ctrl Pts',(0.765348465884739,1.,-1.91287765805174));
#30656=CARTESIAN_POINT('Ctrl Pts',(0.765066729667095,1.,-1.91906491634197));
#30657=CARTESIAN_POINT('Ctrl Pts',(0.764740025488189,1.,-1.92526263537041));
#30658=CARTESIAN_POINT('Ctrl Pts',(0.764369010673889,1.,-1.93147105496367));
#30659=CARTESIAN_POINT('Ctrl Pts',(0.763954049121393,1.,-1.93768964875867));
#30660=CARTESIAN_POINT('Ctrl Pts',(0.76349533353858,1.,-1.94391746617626));
#30661=CARTESIAN_POINT('Ctrl Pts',(0.762992990878774,1.,-1.95015342590025));
#30662=CARTESIAN_POINT('Ctrl Pts',(0.762447203806263,1.,-1.95639665309893));
#30663=CARTESIAN_POINT('Ctrl Pts',(0.761858300014575,1.,-1.96264672744229));
#30664=CARTESIAN_POINT('Ctrl Pts',(0.761226690483986,1.,-1.96890351582545));
#30665=CARTESIAN_POINT('Ctrl Pts',(0.760552825409855,1.,-1.97516705321521));
#30666=CARTESIAN_POINT('Ctrl Pts',(0.759837147452135,1.,-1.98143741418156));
#30667=CARTESIAN_POINT('Ctrl Pts',(0.759080037802242,1.,-1.98771456680806));
#30668=CARTESIAN_POINT('Ctrl Pts',(0.758281796766377,1.,-1.9939983109871));
#30669=CARTESIAN_POINT('Ctrl Pts',(0.757442676862341,1.,-2.00028834739072));
#30670=CARTESIAN_POINT('Ctrl Pts',(0.756562904646496,1.,-2.00658431587682));
#30671=CARTESIAN_POINT('Ctrl Pts',(0.7556427049581,1.,-2.01288584328149));
#30672=CARTESIAN_POINT('Ctrl Pts',(0.75468233072352,1.,-2.01919259406003));
#30673=CARTESIAN_POINT('Ctrl Pts',(0.753682061113765,1.,-2.02550428623587));
#30674=CARTESIAN_POINT('Ctrl Pts',(0.752642180488104,1.,-2.03182068456467));
#30675=CARTESIAN_POINT('Ctrl Pts',(0.751562963361383,1.,-2.03814160092173));
#30676=CARTESIAN_POINT('Ctrl Pts',(0.750444657874758,1.,-2.04446689147754));
#30677=CARTESIAN_POINT('Ctrl Pts',(0.749287468663053,1.,-2.05079645591606));
#30678=CARTESIAN_POINT('Ctrl Pts',(0.748091554181101,1.,-2.05713023030263));
#30679=CARTESIAN_POINT('Ctrl Pts',(0.747103932785504,1.,-2.06220058927162));
#30680=CARTESIAN_POINT('Ctrl Pts',(0.746345871542695,1.,-2.06600523016401));
#30681=CARTESIAN_POINT('Ctrl Pts',(0.74583279137781,1.,-2.06854248895575));
#30682=CARTESIAN_POINT('Ctrl Pts',(0.745574324794401,1.,-2.0698113262342));
#30683=CARTESIAN_POINT('',(0.693717979106306,0.,-1.60662857109684));
#30684=CARTESIAN_POINT('Origin',(0.,0.,0.));
#30685=CARTESIAN_POINT('',(0.892032620296855,1.,-1.5055822144029));
#30686=CARTESIAN_POINT('Origin',(0.,1.,0.));
#30687=CARTESIAN_POINT('',(0.892032620296855,0.,-1.5055822144029));
#30688=CARTESIAN_POINT('Ctrl Pts',(1.23627494547115,-1.,-1.81978687191668));
#30689=CARTESIAN_POINT('Ctrl Pts',(1.23627494547115,1.,-1.81978687191668));
#30690=CARTESIAN_POINT('Ctrl Pts',(1.23509651170476,-1.,-1.81925017193666));
#30691=CARTESIAN_POINT('Ctrl Pts',(1.23509651170476,1.,-1.81925017193666));
#30692=CARTESIAN_POINT('Ctrl Pts',(1.2327422452705,-1.,-1.81817389921279));
#30693=CARTESIAN_POINT('Ctrl Pts',(1.2327422452705,1.,-1.81817389921279));
#30694=CARTESIAN_POINT('Ctrl Pts',(1.2292186489137,-1.,-1.8165508718364));
#30695=CARTESIAN_POINT('Ctrl Pts',(1.2292186489137,1.,-1.8165508718364));
#30696=CARTESIAN_POINT('Ctrl Pts',(1.2245361330495,-1.,-1.81436959210434));
#30697=CARTESIAN_POINT('Ctrl Pts',(1.2245361330495,1.,-1.81436959210434));
#30698=CARTESIAN_POINT('Ctrl Pts',(1.21870906103557,-1.,-1.81161420806656));
#30699=CARTESIAN_POINT('Ctrl Pts',(1.21870906103557,1.,-1.81161420806656));
#30700=CARTESIAN_POINT('Ctrl Pts',(1.21290815708314,-1.,-1.80882996917129));
#30701=CARTESIAN_POINT('Ctrl Pts',(1.21290815708314,1.,-1.80882996917129));
#30702=CARTESIAN_POINT('Ctrl Pts',(1.20713356605475,-1.,-1.80601678480707));
#30703=CARTESIAN_POINT('Ctrl Pts',(1.20713356605475,1.,-1.80601678480707));
#30704=CARTESIAN_POINT('Ctrl Pts',(1.20138548938974,-1.,-1.80317454838603));
#30705=CARTESIAN_POINT('Ctrl Pts',(1.20138548938974,1.,-1.80317454838603));
#30706=CARTESIAN_POINT('Ctrl Pts',(1.19566418930242,-1.,-1.80030314369879));
#30707=CARTESIAN_POINT('Ctrl Pts',(1.19566418930242,1.,-1.80030314369879));
#30708=CARTESIAN_POINT('Ctrl Pts',(1.18996997934445,-1.,-1.79740245923478));
#30709=CARTESIAN_POINT('Ctrl Pts',(1.18996997934445,1.,-1.79740245923478));
#30710=CARTESIAN_POINT('Ctrl Pts',(1.18430321697432,-1.,-1.79447240321515));
#30711=CARTESIAN_POINT('Ctrl Pts',(1.18430321697432,1.,-1.79447240321515));
#30712=CARTESIAN_POINT('Ctrl Pts',(1.17866429440809,-1.,-1.79151291552689));
#30713=CARTESIAN_POINT('Ctrl Pts',(1.17866429440809,1.,-1.79151291552689));
#30714=CARTESIAN_POINT('Ctrl Pts',(1.17305363177328,-1.,-1.78852398877617));
#30715=CARTESIAN_POINT('Ctrl Pts',(1.17305363177328,1.,-1.78852398877617));
#30716=CARTESIAN_POINT('Ctrl Pts',(1.16747166312303,-1.,-1.78550566040443));
#30717=CARTESIAN_POINT('Ctrl Pts',(1.16747166312303,1.,-1.78550566040443));
#30718=CARTESIAN_POINT('Ctrl Pts',(1.16191881298499,-1.,-1.78245795881009));
#30719=CARTESIAN_POINT('Ctrl Pts',(1.16191881298499,1.,-1.78245795881009));
#30720=CARTESIAN_POINT('Ctrl Pts',(1.15639547194698,-1.,-1.77938085564275));
#30721=CARTESIAN_POINT('Ctrl Pts',(1.15639547194698,1.,-1.77938085564275));
#30722=CARTESIAN_POINT('Ctrl Pts',(1.15090197841514,-1.,-1.7762742255701));
#30723=CARTESIAN_POINT('Ctrl Pts',(1.15090197841514,1.,-1.7762742255701));
#30724=CARTESIAN_POINT('Ctrl Pts',(1.1454385822692,-1.,-1.77313777896194));
#30725=CARTESIAN_POINT('Ctrl Pts',(1.1454385822692,1.,-1.77313777896194));
#30726=CARTESIAN_POINT('Ctrl Pts',(1.14000548336975,-1.,-1.76997111386769));
#30727=CARTESIAN_POINT('Ctrl Pts',(1.14000548336975,1.,-1.76997111386769));
#30728=CARTESIAN_POINT('Ctrl Pts',(1.1346029180462,-1.,-1.76677384551862));
#30729=CARTESIAN_POINT('Ctrl Pts',(1.1346029180462,1.,-1.76677384551862));
#30730=CARTESIAN_POINT('Ctrl Pts',(1.12923123555075,-1.,-1.7635457196617));
#30731=CARTESIAN_POINT('Ctrl Pts',(1.12923123555075,1.,-1.7635457196617));
#30732=CARTESIAN_POINT('Ctrl Pts',(1.12389096855086,-1.,-1.76028671825096));
#30733=CARTESIAN_POINT('Ctrl Pts',(1.12389096855086,1.,-1.76028671825096));
#30734=CARTESIAN_POINT('Ctrl Pts',(1.11858293216763,-1.,-1.75699720772105));
#30735=CARTESIAN_POINT('Ctrl Pts',(1.11858293216763,1.,-1.75699720772105));
#30736=CARTESIAN_POINT('Ctrl Pts',(1.11330807582551,-1.,-1.7536777209463));
#30737=CARTESIAN_POINT('Ctrl Pts',(1.11330807582551,1.,-1.7536777209463));
#30738=CARTESIAN_POINT('Ctrl Pts',(1.10806728183007,-1.,-1.7503286607592));
#30739=CARTESIAN_POINT('Ctrl Pts',(1.10806728183007,1.,-1.7503286607592));
#30740=CARTESIAN_POINT('Ctrl Pts',(1.10286118991143,-1.,-1.74695004214923));
#30741=CARTESIAN_POINT('Ctrl Pts',(1.10286118991143,1.,-1.74695004214923));
#30742=CARTESIAN_POINT('Ctrl Pts',(1.09768999241225,-1.,-1.74354119236208));
#30743=CARTESIAN_POINT('Ctrl Pts',(1.09768999241225,1.,-1.74354119236208));
#30744=CARTESIAN_POINT('Ctrl Pts',(1.09255329056493,-1.,-1.74010053962247));
#30745=CARTESIAN_POINT('Ctrl Pts',(1.09255329056493,1.,-1.74010053962247));
#30746=CARTESIAN_POINT('Ctrl Pts',(1.08745056285427,-1.,-1.73662628326091));
#30747=CARTESIAN_POINT('Ctrl Pts',(1.08745056285427,1.,-1.73662628326091));
#30748=CARTESIAN_POINT('Ctrl Pts',(1.08238162784749,-1.,-1.73311705663407));
#30749=CARTESIAN_POINT('Ctrl Pts',(1.08238162784749,1.,-1.73311705663407));
#30750=CARTESIAN_POINT('Ctrl Pts',(1.0773470373727,-1.,-1.72957248977424));
#30751=CARTESIAN_POINT('Ctrl Pts',(1.0773470373727,1.,-1.72957248977424));
#30752=CARTESIAN_POINT('Ctrl Pts',(1.07234866990252,-1.,-1.72599406198488));
#30753=CARTESIAN_POINT('Ctrl Pts',(1.07234866990252,1.,-1.72599406198488));
#30754=CARTESIAN_POINT('Ctrl Pts',(1.06738966975462,-1.,-1.72238500928453));
#30755=CARTESIAN_POINT('Ctrl Pts',(1.06738966975462,1.,-1.72238500928453));
#30756=CARTESIAN_POINT('Ctrl Pts',(1.06247324680647,-1.,-1.71874858456904));
#30757=CARTESIAN_POINT('Ctrl Pts',(1.06247324680647,1.,-1.71874858456904));
#30758=CARTESIAN_POINT('Ctrl Pts',(1.05760163192479,-1.,-1.7150865442702));
#30759=CARTESIAN_POINT('Ctrl Pts',(1.05760163192479,1.,-1.7150865442702));
#30760=CARTESIAN_POINT('Ctrl Pts',(1.05277517202855,-1.,-1.71139783543989));
#30761=CARTESIAN_POINT('Ctrl Pts',(1.05277517202855,1.,-1.71139783543989));
#30762=CARTESIAN_POINT('Ctrl Pts',(1.04799085404995,-1.,-1.70767646263649));
#30763=CARTESIAN_POINT('Ctrl Pts',(1.04799085404995,1.,-1.70767646263649));
#30764=CARTESIAN_POINT('Ctrl Pts',(1.04324363334554,-1.,-1.70391338707982));
#30765=CARTESIAN_POINT('Ctrl Pts',(1.04324363334554,1.,-1.70391338707982));
#30766=CARTESIAN_POINT('Ctrl Pts',(1.03852922490789,-1.,-1.70010052930962));
#30767=CARTESIAN_POINT('Ctrl Pts',(1.03852922490789,1.,-1.70010052930962));
#30768=CARTESIAN_POINT('Ctrl Pts',(1.03384646003588,-1.,-1.69623414782771));
#30769=CARTESIAN_POINT('Ctrl Pts',(1.03384646003588,1.,-1.69623414782771));
#30770=CARTESIAN_POINT('Ctrl Pts',(1.02919977579147,-1.,-1.69231840863458));
#30771=CARTESIAN_POINT('Ctrl Pts',(1.02919977579147,1.,-1.69231840863458));
#30772=CARTESIAN_POINT('Ctrl Pts',(1.02460180535255,-1.,-1.68836910178447));
#30773=CARTESIAN_POINT('Ctrl Pts',(1.02460180535255,1.,-1.68836910178447));
#30774=CARTESIAN_POINT('Ctrl Pts',(1.02006795074201,-1.,-1.68440578021706));
#30775=CARTESIAN_POINT('Ctrl Pts',(1.02006795074201,1.,-1.68440578021706));
#30776=CARTESIAN_POINT('Ctrl Pts',(1.01561026162773,-1.,-1.68044289894798));
#30777=CARTESIAN_POINT('Ctrl Pts',(1.01561026162773,1.,-1.68044289894798));
#30778=CARTESIAN_POINT('Ctrl Pts',(1.01123236493511,-1.,-1.67648246776464));
#30779=CARTESIAN_POINT('Ctrl Pts',(1.01123236493511,1.,-1.67648246776464));
#30780=CARTESIAN_POINT('Ctrl Pts',(1.00692206696414,-1.,-1.67250335383293));
#30781=CARTESIAN_POINT('Ctrl Pts',(1.00692206696414,1.,-1.67250335383293));
#30782=CARTESIAN_POINT('Ctrl Pts',(1.00265091003727,-1.,-1.66846059277303));
#30783=CARTESIAN_POINT('Ctrl Pts',(1.00265091003727,1.,-1.66846059277303));
#30784=CARTESIAN_POINT('Ctrl Pts',(0.998389654952757,-1.,-1.66430758030376));
#30785=CARTESIAN_POINT('Ctrl Pts',(0.998389654952757,1.,-1.66430758030376));
#30786=CARTESIAN_POINT('Ctrl Pts',(0.994121836661305,-1.,-1.66001553809947));
#30787=CARTESIAN_POINT('Ctrl Pts',(0.994121836661305,1.,-1.66001553809947));
#30788=CARTESIAN_POINT('Ctrl Pts',(0.989855627854164,-1.,-1.65559044289699));
#30789=CARTESIAN_POINT('Ctrl Pts',(0.989855627854164,1.,-1.65559044289699));
#30790=CARTESIAN_POINT('Ctrl Pts',(0.98564262292082,-1.,-1.65110016612638));
#30791=CARTESIAN_POINT('Ctrl Pts',(0.98564262292082,1.,-1.65110016612638));
#30792=CARTESIAN_POINT('Ctrl Pts',(0.981562530939489,-1.,-1.64665139190656));
#30793=CARTESIAN_POINT('Ctrl Pts',(0.981562530939489,1.,-1.64665139190656));
#30794=CARTESIAN_POINT('Ctrl Pts',(0.977689794119416,-1.,-1.64233990826687));
#30795=CARTESIAN_POINT('Ctrl Pts',(0.977689794119416,1.,-1.64233990826687));
#30796=CARTESIAN_POINT('Ctrl Pts',(0.974066058287418,-1.,-1.63820952658144));
#30797=CARTESIAN_POINT('Ctrl Pts',(0.974066058287418,1.,-1.63820952658144));
#30798=CARTESIAN_POINT('Ctrl Pts',(0.970669715997509,-1.,-1.63420665729798));
#30799=CARTESIAN_POINT('Ctrl Pts',(0.970669715997509,1.,-1.63420665729798));
#30800=CARTESIAN_POINT('Ctrl Pts',(0.967387853230345,-1.,-1.63013849959462));
#30801=CARTESIAN_POINT('Ctrl Pts',(0.967387853230345,1.,-1.63013849959462));
#30802=CARTESIAN_POINT('Ctrl Pts',(0.964046107040535,-1.,-1.62571930670187));
#30803=CARTESIAN_POINT('Ctrl Pts',(0.964046107040535,1.,-1.62571930670187));
#30804=CARTESIAN_POINT('Ctrl Pts',(0.960438326101728,-1.,-1.62061638140221));
#30805=CARTESIAN_POINT('Ctrl Pts',(0.960438326101728,1.,-1.62061638140221));
#30806=CARTESIAN_POINT('Ctrl Pts',(0.95635442292067,-1.,-1.61449324337085));
#30807=CARTESIAN_POINT('Ctrl Pts',(0.95635442292067,1.,-1.61449324337085));
#30808=CARTESIAN_POINT('Ctrl Pts',(0.951613284356035,-1.,-1.60706069896936));
#30809=CARTESIAN_POINT('Ctrl Pts',(0.951613284356035,1.,-1.60706069896936));
#30810=CARTESIAN_POINT('Ctrl Pts',(0.946078063315257,-1.,-1.59810042043673));
#30811=CARTESIAN_POINT('Ctrl Pts',(0.946078063315257,1.,-1.59810042043673));
#30812=CARTESIAN_POINT('Ctrl Pts',(0.939646377893399,-1.,-1.58744937487176));
#30813=CARTESIAN_POINT('Ctrl Pts',(0.939646377893399,1.,-1.58744937487176));
#30814=CARTESIAN_POINT('Ctrl Pts',(0.932246680108685,-1.,-1.57499388382243));
#30815=CARTESIAN_POINT('Ctrl Pts',(0.932246680108685,1.,-1.57499388382243));
#30816=CARTESIAN_POINT('Ctrl Pts',(0.923832188944341,-1.,-1.56065988578893));
#30817=CARTESIAN_POINT('Ctrl Pts',(0.923832188944341,1.,-1.56065988578893));
#30818=CARTESIAN_POINT('Ctrl Pts',(0.914375919026456,-1.,-1.54440491149498));
#30819=CARTESIAN_POINT('Ctrl Pts',(0.914375919026456,1.,-1.54440491149498));
#30820=CARTESIAN_POINT('Ctrl Pts',(0.905967409625651,-1.,-1.52984849887993));
#30821=CARTESIAN_POINT('Ctrl Pts',(0.905967409625651,1.,-1.52984849887993));
#30822=CARTESIAN_POINT('Ctrl Pts',(0.89918504748351,-1.,-1.51805569590094));
#30823=CARTESIAN_POINT('Ctrl Pts',(0.89918504748351,1.,-1.51805569590094));
#30824=CARTESIAN_POINT('Ctrl Pts',(0.894452006964543,-1.,-1.50980486806688));
#30825=CARTESIAN_POINT('Ctrl Pts',(0.894452006964543,1.,-1.50980486806688));
#30826=CARTESIAN_POINT('Ctrl Pts',(0.892032620296855,-1.,-1.5055822144029));
#30827=CARTESIAN_POINT('Ctrl Pts',(0.892032620296855,1.,-1.5055822144029));
#30828=CARTESIAN_POINT('',(1.23627494547115,1.,-1.81978687191668));
#30829=CARTESIAN_POINT('Ctrl Pts',(1.23627494547115,1.,-1.81978687191668));
#30830=CARTESIAN_POINT('Ctrl Pts',(1.23509651170476,1.,-1.81925017193666));
#30831=CARTESIAN_POINT('Ctrl Pts',(1.2327422452705,1.,-1.81817389921279));
#30832=CARTESIAN_POINT('Ctrl Pts',(1.2292186489137,1.,-1.8165508718364));
#30833=CARTESIAN_POINT('Ctrl Pts',(1.2245361330495,1.,-1.81436959210434));
#30834=CARTESIAN_POINT('Ctrl Pts',(1.21870906103557,1.,-1.81161420806656));
#30835=CARTESIAN_POINT('Ctrl Pts',(1.21290815708314,1.,-1.80882996917129));
#30836=CARTESIAN_POINT('Ctrl Pts',(1.20713356605475,1.,-1.80601678480707));
#30837=CARTESIAN_POINT('Ctrl Pts',(1.20138548938974,1.,-1.80317454838603));
#30838=CARTESIAN_POINT('Ctrl Pts',(1.19566418930242,1.,-1.80030314369879));
#30839=CARTESIAN_POINT('Ctrl Pts',(1.18996997934445,1.,-1.79740245923478));
#30840=CARTESIAN_POINT('Ctrl Pts',(1.18430321697432,1.,-1.79447240321515));
#30841=CARTESIAN_POINT('Ctrl Pts',(1.17866429440809,1.,-1.79151291552689));
#30842=CARTESIAN_POINT('Ctrl Pts',(1.17305363177328,1.,-1.78852398877617));
#30843=CARTESIAN_POINT('Ctrl Pts',(1.16747166312303,1.,-1.78550566040443));
#30844=CARTESIAN_POINT('Ctrl Pts',(1.16191881298499,1.,-1.78245795881009));
#30845=CARTESIAN_POINT('Ctrl Pts',(1.15639547194698,1.,-1.77938085564275));
#30846=CARTESIAN_POINT('Ctrl Pts',(1.15090197841514,1.,-1.7762742255701));
#30847=CARTESIAN_POINT('Ctrl Pts',(1.1454385822692,1.,-1.77313777896194));
#30848=CARTESIAN_POINT('Ctrl Pts',(1.14000548336975,1.,-1.76997111386769));
#30849=CARTESIAN_POINT('Ctrl Pts',(1.1346029180462,1.,-1.76677384551862));
#30850=CARTESIAN_POINT('Ctrl Pts',(1.12923123555075,1.,-1.7635457196617));
#30851=CARTESIAN_POINT('Ctrl Pts',(1.12389096855086,1.,-1.76028671825096));
#30852=CARTESIAN_POINT('Ctrl Pts',(1.11858293216763,1.,-1.75699720772105));
#30853=CARTESIAN_POINT('Ctrl Pts',(1.11330807582551,1.,-1.7536777209463));
#30854=CARTESIAN_POINT('Ctrl Pts',(1.10806728183007,1.,-1.7503286607592));
#30855=CARTESIAN_POINT('Ctrl Pts',(1.10286118991143,1.,-1.74695004214923));
#30856=CARTESIAN_POINT('Ctrl Pts',(1.09768999241225,1.,-1.74354119236208));
#30857=CARTESIAN_POINT('Ctrl Pts',(1.09255329056493,1.,-1.74010053962247));
#30858=CARTESIAN_POINT('Ctrl Pts',(1.08745056285427,1.,-1.73662628326091));
#30859=CARTESIAN_POINT('Ctrl Pts',(1.08238162784749,1.,-1.73311705663407));
#30860=CARTESIAN_POINT('Ctrl Pts',(1.0773470373727,1.,-1.72957248977424));
#30861=CARTESIAN_POINT('Ctrl Pts',(1.07234866990252,1.,-1.72599406198488));
#30862=CARTESIAN_POINT('Ctrl Pts',(1.06738966975462,1.,-1.72238500928453));
#30863=CARTESIAN_POINT('Ctrl Pts',(1.06247324680647,1.,-1.71874858456904));
#30864=CARTESIAN_POINT('Ctrl Pts',(1.05760163192479,1.,-1.7150865442702));
#30865=CARTESIAN_POINT('Ctrl Pts',(1.05277517202855,1.,-1.71139783543989));
#30866=CARTESIAN_POINT('Ctrl Pts',(1.04799085404995,1.,-1.70767646263649));
#30867=CARTESIAN_POINT('Ctrl Pts',(1.04324363334554,1.,-1.70391338707982));
#30868=CARTESIAN_POINT('Ctrl Pts',(1.03852922490789,1.,-1.70010052930962));
#30869=CARTESIAN_POINT('Ctrl Pts',(1.03384646003588,1.,-1.69623414782771));
#30870=CARTESIAN_POINT('Ctrl Pts',(1.02919977579147,1.,-1.69231840863458));
#30871=CARTESIAN_POINT('Ctrl Pts',(1.02460180535255,1.,-1.68836910178447));
#30872=CARTESIAN_POINT('Ctrl Pts',(1.02006795074201,1.,-1.68440578021706));
#30873=CARTESIAN_POINT('Ctrl Pts',(1.01561026162773,1.,-1.68044289894798));
#30874=CARTESIAN_POINT('Ctrl Pts',(1.01123236493511,1.,-1.67648246776464));
#30875=CARTESIAN_POINT('Ctrl Pts',(1.00692206696414,1.,-1.67250335383293));
#30876=CARTESIAN_POINT('Ctrl Pts',(1.00265091003727,1.,-1.66846059277303));
#30877=CARTESIAN_POINT('Ctrl Pts',(0.998389654952757,1.,-1.66430758030376));
#30878=CARTESIAN_POINT('Ctrl Pts',(0.994121836661305,1.,-1.66001553809947));
#30879=CARTESIAN_POINT('Ctrl Pts',(0.989855627854164,1.,-1.65559044289699));
#30880=CARTESIAN_POINT('Ctrl Pts',(0.98564262292082,1.,-1.65110016612638));
#30881=CARTESIAN_POINT('Ctrl Pts',(0.981562530939489,1.,-1.64665139190656));
#30882=CARTESIAN_POINT('Ctrl Pts',(0.977689794119416,1.,-1.64233990826687));
#30883=CARTESIAN_POINT('Ctrl Pts',(0.974066058287418,1.,-1.63820952658144));
#30884=CARTESIAN_POINT('Ctrl Pts',(0.970669715997509,1.,-1.63420665729798));
#30885=CARTESIAN_POINT('Ctrl Pts',(0.967387853230345,1.,-1.63013849959462));
#30886=CARTESIAN_POINT('Ctrl Pts',(0.964046107040535,1.,-1.62571930670187));
#30887=CARTESIAN_POINT('Ctrl Pts',(0.960438326101728,1.,-1.62061638140221));
#30888=CARTESIAN_POINT('Ctrl Pts',(0.95635442292067,1.,-1.61449324337085));
#30889=CARTESIAN_POINT('Ctrl Pts',(0.951613284356035,1.,-1.60706069896936));
#30890=CARTESIAN_POINT('Ctrl Pts',(0.946078063315257,1.,-1.59810042043673));
#30891=CARTESIAN_POINT('Ctrl Pts',(0.939646377893399,1.,-1.58744937487176));
#30892=CARTESIAN_POINT('Ctrl Pts',(0.932246680108685,1.,-1.57499388382243));
#30893=CARTESIAN_POINT('Ctrl Pts',(0.923832188944341,1.,-1.56065988578893));
#30894=CARTESIAN_POINT('Ctrl Pts',(0.914375919026456,1.,-1.54440491149498));
#30895=CARTESIAN_POINT('Ctrl Pts',(0.905967409625651,1.,-1.52984849887993));
#30896=CARTESIAN_POINT('Ctrl Pts',(0.89918504748351,1.,-1.51805569590094));
#30897=CARTESIAN_POINT('Ctrl Pts',(0.894452006964543,1.,-1.50980486806688));
#30898=CARTESIAN_POINT('Ctrl Pts',(0.892032620296855,1.,-1.5055822144029));
#30899=CARTESIAN_POINT('',(1.23627494547115,0.,-1.81978687191668));
#30900=CARTESIAN_POINT('Origin',(1.34869019493419,0.,-1.73811241238545));
#30901=CARTESIAN_POINT('',(1.34869019493419,1.,-1.73811241238545));
#30902=CARTESIAN_POINT('',(1.23627494547115,1.,-1.81978687191668));
#30903=CARTESIAN_POINT('',(1.34869019493419,0.,-1.73811241238545));
#30904=CARTESIAN_POINT('Ctrl Pts',(1.15624053661742,-1.,-1.31362392696032));
#30905=CARTESIAN_POINT('Ctrl Pts',(1.15624053661742,1.,-1.31362392696032));
#30906=CARTESIAN_POINT('Ctrl Pts',(1.15950888730809,-1.,-1.31722977216397));
#30907=CARTESIAN_POINT('Ctrl Pts',(1.15950888730809,1.,-1.31722977216397));
#30908=CARTESIAN_POINT('Ctrl Pts',(1.16589330093588,-1.,-1.32428080721772));
#30909=CARTESIAN_POINT('Ctrl Pts',(1.16589330093588,1.,-1.32428080721772));
#30910=CARTESIAN_POINT('Ctrl Pts',(1.17501305789857,-1.,-1.33437539347008));
#30911=CARTESIAN_POINT('Ctrl Pts',(1.17501305789857,1.,-1.33437539347008));
#30912=CARTESIAN_POINT('Ctrl Pts',(1.18625865667441,-1.,-1.34687054001093));
#30913=CARTESIAN_POINT('Ctrl Pts',(1.18625865667441,1.,-1.34687054001093));
#30914=CARTESIAN_POINT('Ctrl Pts',(1.1987959077932,-1.,-1.36088705043885));
#30915=CARTESIAN_POINT('Ctrl Pts',(1.1987959077932,1.,-1.36088705043885));
#30916=CARTESIAN_POINT('Ctrl Pts',(1.20982812925645,-1.,-1.37331915607905));
#30917=CARTESIAN_POINT('Ctrl Pts',(1.20982812925645,1.,-1.37331915607905));
#30918=CARTESIAN_POINT('Ctrl Pts',(1.21938737280852,-1.,-1.38420564527715));
#30919=CARTESIAN_POINT('Ctrl Pts',(1.21938737280852,1.,-1.38420564527715));
#30920=CARTESIAN_POINT('Ctrl Pts',(1.22752961899387,-1.,-1.39361389568796));
#30921=CARTESIAN_POINT('Ctrl Pts',(1.22752961899387,1.,-1.39361389568796));
#30922=CARTESIAN_POINT('Ctrl Pts',(1.23434087290423,-1.,-1.40164708206106));
#30923=CARTESIAN_POINT('Ctrl Pts',(1.23434087290423,1.,-1.40164708206106));
#30924=CARTESIAN_POINT('Ctrl Pts',(1.23994455029534,-1.,-1.40845295531283));
#30925=CARTESIAN_POINT('Ctrl Pts',(1.23994455029534,1.,-1.40845295531283));
#30926=CARTESIAN_POINT('Ctrl Pts',(1.24450600513056,-1.,-1.41422913175179));
#30927=CARTESIAN_POINT('Ctrl Pts',(1.24450600513056,1.,-1.41422913175179));
#30928=CARTESIAN_POINT('Ctrl Pts',(1.24824430986571,-1.,-1.41923722596025));
#30929=CARTESIAN_POINT('Ctrl Pts',(1.24824430986571,1.,-1.41923722596025));
#30930=CARTESIAN_POINT('Ctrl Pts',(1.2514145557001,-1.,-1.42378102115575));
#30931=CARTESIAN_POINT('Ctrl Pts',(1.2514145557001,1.,-1.42378102115575));
#30932=CARTESIAN_POINT('Ctrl Pts',(1.25426945222639,-1.,-1.42815938799387));
#30933=CARTESIAN_POINT('Ctrl Pts',(1.25426945222639,1.,-1.42815938799387));
#30934=CARTESIAN_POINT('Ctrl Pts',(1.25702687965755,-1.,-1.43262645609691));
#30935=CARTESIAN_POINT('Ctrl Pts',(1.25702687965755,1.,-1.43262645609691));
#30936=CARTESIAN_POINT('Ctrl Pts',(1.25983531012005,-1.,-1.43734919180848));
#30937=CARTESIAN_POINT('Ctrl Pts',(1.25983531012005,1.,-1.43734919180848));
#30938=CARTESIAN_POINT('Ctrl Pts',(1.26273903323858,-1.,-1.44236470511303));
#30939=CARTESIAN_POINT('Ctrl Pts',(1.26273903323858,1.,-1.44236470511303));
#30940=CARTESIAN_POINT('Ctrl Pts',(1.26570925118868,-1.,-1.44761985001662));
#30941=CARTESIAN_POINT('Ctrl Pts',(1.26570925118868,1.,-1.44761985001662));
#30942=CARTESIAN_POINT('Ctrl Pts',(1.2686778680489,-1.,-1.45301422764247));
#30943=CARTESIAN_POINT('Ctrl Pts',(1.2686778680489,1.,-1.45301422764247));
#30944=CARTESIAN_POINT('Ctrl Pts',(1.27156805265289,-1.,-1.45843906294697));
#30945=CARTESIAN_POINT('Ctrl Pts',(1.27156805265289,1.,-1.45843906294697));
#30946=CARTESIAN_POINT('Ctrl Pts',(1.27433119897822,-1.,-1.46382431332476));
#30947=CARTESIAN_POINT('Ctrl Pts',(1.27433119897822,1.,-1.46382431332476));
#30948=CARTESIAN_POINT('Ctrl Pts',(1.27696414831089,-1.,-1.46916035917133));
#30949=CARTESIAN_POINT('Ctrl Pts',(1.27696414831089,1.,-1.46916035917133));
#30950=CARTESIAN_POINT('Ctrl Pts',(1.2794891824849,-1.,-1.4744717526707));
#30951=CARTESIAN_POINT('Ctrl Pts',(1.2794891824849,1.,-1.4744717526707));
#30952=CARTESIAN_POINT('Ctrl Pts',(1.28194158939517,-1.,-1.47980070347096));
#30953=CARTESIAN_POINT('Ctrl Pts',(1.28194158939517,1.,-1.47980070347096));
#30954=CARTESIAN_POINT('Ctrl Pts',(1.28435533880201,-1.,-1.4851881711891));
#30955=CARTESIAN_POINT('Ctrl Pts',(1.28435533880201,1.,-1.4851881711891));
#30956=CARTESIAN_POINT('Ctrl Pts',(1.2867467611644,-1.,-1.4906522831278));
#30957=CARTESIAN_POINT('Ctrl Pts',(1.2867467611644,1.,-1.4906522831278));
#30958=CARTESIAN_POINT('Ctrl Pts',(1.28911506584254,-1.,-1.49618896881754));
#30959=CARTESIAN_POINT('Ctrl Pts',(1.28911506584254,1.,-1.49618896881754));
#30960=CARTESIAN_POINT('Ctrl Pts',(1.29145022885181,-1.,-1.50178230149776));
#30961=CARTESIAN_POINT('Ctrl Pts',(1.29145022885181,1.,-1.50178230149776));
#30962=CARTESIAN_POINT('Ctrl Pts',(1.29373841372842,-1.,-1.50741159078365));
#30963=CARTESIAN_POINT('Ctrl Pts',(1.29373841372842,1.,-1.50741159078365));
#30964=CARTESIAN_POINT('Ctrl Pts',(1.29596850710509,-1.,-1.51305994241402));
#30965=CARTESIAN_POINT('Ctrl Pts',(1.29596850710509,1.,-1.51305994241402));
#30966=CARTESIAN_POINT('Ctrl Pts',(1.29813791800747,-1.,-1.51872184912724));
#30967=CARTESIAN_POINT('Ctrl Pts',(1.29813791800747,1.,-1.51872184912724));
#30968=CARTESIAN_POINT('Ctrl Pts',(1.30024984366328,-1.,-1.52439957861062));
#30969=CARTESIAN_POINT('Ctrl Pts',(1.30024984366328,1.,-1.52439957861062));
#30970=CARTESIAN_POINT('Ctrl Pts',(1.30231064395568,-1.,-1.53009970283891));
#30971=CARTESIAN_POINT('Ctrl Pts',(1.30231064395568,1.,-1.53009970283891));
#30972=CARTESIAN_POINT('Ctrl Pts',(1.30432735639489,-1.,-1.53582981268977));
#30973=CARTESIAN_POINT('Ctrl Pts',(1.30432735639489,1.,-1.53582981268977));
#30974=CARTESIAN_POINT('Ctrl Pts',(1.30630475189556,-1.,-1.54159462645432));
#30975=CARTESIAN_POINT('Ctrl Pts',(1.30630475189556,1.,-1.54159462645432));
#30976=CARTESIAN_POINT('Ctrl Pts',(1.30824393907473,-1.,-1.54739413957185));
#30977=CARTESIAN_POINT('Ctrl Pts',(1.30824393907473,1.,-1.54739413957185));
#30978=CARTESIAN_POINT('Ctrl Pts',(1.31014393684222,-1.,-1.55322568759481));
#30979=CARTESIAN_POINT('Ctrl Pts',(1.31014393684222,1.,-1.55322568759481));
#30980=CARTESIAN_POINT('Ctrl Pts',(1.31200264341696,-1.,-1.55908521254821));
#30981=CARTESIAN_POINT('Ctrl Pts',(1.31200264341696,1.,-1.55908521254821));
#30982=CARTESIAN_POINT('Ctrl Pts',(1.31381795281002,-1.,-1.56496872402353));
#30983=CARTESIAN_POINT('Ctrl Pts',(1.31381795281002,1.,-1.56496872402353));
#30984=CARTESIAN_POINT('Ctrl Pts',(1.31558903860016,-1.,-1.57087397835723));
#30985=CARTESIAN_POINT('Ctrl Pts',(1.31558903860016,1.,-1.57087397835723));
#30986=CARTESIAN_POINT('Ctrl Pts',(1.31731642317187,-1.,-1.5768005650559));
#30987=CARTESIAN_POINT('Ctrl Pts',(1.31731642317187,1.,-1.5768005650559));
#30988=CARTESIAN_POINT('Ctrl Pts',(1.31900135021432,-1.,-1.58274907898834));
#30989=CARTESIAN_POINT('Ctrl Pts',(1.31900135021432,1.,-1.58274907898834));
#30990=CARTESIAN_POINT('Ctrl Pts',(1.32064537110892,-1.,-1.58872057258245));
#30991=CARTESIAN_POINT('Ctrl Pts',(1.32064537110892,1.,-1.58872057258245));
#30992=CARTESIAN_POINT('Ctrl Pts',(1.32224985747682,-1.,-1.59471591079403));
#30993=CARTESIAN_POINT('Ctrl Pts',(1.32224985747682,1.,-1.59471591079403));
#30994=CARTESIAN_POINT('Ctrl Pts',(1.32381550858256,-1.,-1.60073511858687));
#30995=CARTESIAN_POINT('Ctrl Pts',(1.32381550858256,1.,-1.60073511858687));
#30996=CARTESIAN_POINT('Ctrl Pts',(1.32534250785782,-1.,-1.60677758290954));
#30997=CARTESIAN_POINT('Ctrl Pts',(1.32534250785782,1.,-1.60677758290954));
#30998=CARTESIAN_POINT('Ctrl Pts',(1.32683074483356,-1.,-1.6128423401575));
#30999=CARTESIAN_POINT('Ctrl Pts',(1.32683074483356,1.,-1.6128423401575));
#31000=CARTESIAN_POINT('Ctrl Pts',(1.32828000610449,-1.,-1.61892832270724));
#31001=CARTESIAN_POINT('Ctrl Pts',(1.32828000610449,1.,-1.61892832270724));
#31002=CARTESIAN_POINT('Ctrl Pts',(1.3296901950568,-1.,-1.62503464209797));
#31003=CARTESIAN_POINT('Ctrl Pts',(1.3296901950568,1.,-1.62503464209797));
#31004=CARTESIAN_POINT('Ctrl Pts',(1.33106149345645,-1.,-1.63116079730923));
#31005=CARTESIAN_POINT('Ctrl Pts',(1.33106149345645,1.,-1.63116079730923));
#31006=CARTESIAN_POINT('Ctrl Pts',(1.33239425103724,-1.,-1.63730653475089));
#31007=CARTESIAN_POINT('Ctrl Pts',(1.33239425103724,1.,-1.63730653475089));
#31008=CARTESIAN_POINT('Ctrl Pts',(1.33368890676572,-1.,-1.6434717485603));
#31009=CARTESIAN_POINT('Ctrl Pts',(1.33368890676572,1.,-1.6434717485603));
#31010=CARTESIAN_POINT('Ctrl Pts',(1.33494590467993,-1.,-1.6496563728683));
#31011=CARTESIAN_POINT('Ctrl Pts',(1.33494590467993,1.,-1.6496563728683));
#31012=CARTESIAN_POINT('Ctrl Pts',(1.33616559745172,-1.,-1.65586025952593));
#31013=CARTESIAN_POINT('Ctrl Pts',(1.33616559745172,1.,-1.65586025952593));
#31014=CARTESIAN_POINT('Ctrl Pts',(1.33734820885262,-1.,-1.66208312541983));
#31015=CARTESIAN_POINT('Ctrl Pts',(1.33734820885262,1.,-1.66208312541983));
#31016=CARTESIAN_POINT('Ctrl Pts',(1.33849388654388,-1.,-1.66832460783989));
#31017=CARTESIAN_POINT('Ctrl Pts',(1.33849388654388,1.,-1.66832460783989));
#31018=CARTESIAN_POINT('Ctrl Pts',(1.3396027347034,-1.,-1.67458429426086));
#31019=CARTESIAN_POINT('Ctrl Pts',(1.3396027347034,1.,-1.67458429426086));
#31020=CARTESIAN_POINT('Ctrl Pts',(1.34067485185203,-1.,-1.68086176030362));
#31021=CARTESIAN_POINT('Ctrl Pts',(1.34067485185203,1.,-1.68086176030362));
#31022=CARTESIAN_POINT('Ctrl Pts',(1.341710374848,-1.,-1.68715660868764));
#31023=CARTESIAN_POINT('Ctrl Pts',(1.341710374848,1.,-1.68715660868764));
#31024=CARTESIAN_POINT('Ctrl Pts',(1.34270948206319,-1.,-1.6934684849687));
#31025=CARTESIAN_POINT('Ctrl Pts',(1.34270948206319,1.,-1.6934684849687));
#31026=CARTESIAN_POINT('Ctrl Pts',(1.34367237124483,-1.,-1.69979707754427));
#31027=CARTESIAN_POINT('Ctrl Pts',(1.34367237124483,1.,-1.69979707754427));
#31028=CARTESIAN_POINT('Ctrl Pts',(1.34459924533831,-1.,-1.70614212266738));
#31029=CARTESIAN_POINT('Ctrl Pts',(1.34459924533831,1.,-1.70614212266738));
#31030=CARTESIAN_POINT('Ctrl Pts',(1.34549029589416,-1.,-1.71250340686822));
#31031=CARTESIAN_POINT('Ctrl Pts',(1.34549029589416,1.,-1.71250340686822));
#31032=CARTESIAN_POINT('Ctrl Pts',(1.34634568653227,-1.,-1.7188807715049));
#31033=CARTESIAN_POINT('Ctrl Pts',(1.34634568653227,1.,-1.7188807715049));
#31034=CARTESIAN_POINT('Ctrl Pts',(1.34716554819527,-1.,-1.72527410680674));
#31035=CARTESIAN_POINT('Ctrl Pts',(1.34716554819527,1.,-1.72527410680674));
#31036=CARTESIAN_POINT('Ctrl Pts',(1.34779309152035,-1.,-1.7304014965394));
#31037=CARTESIAN_POINT('Ctrl Pts',(1.34779309152035,1.,-1.7304014965394));
#31038=CARTESIAN_POINT('Ctrl Pts',(1.34824783112887,-1.,-1.73425417885907));
#31039=CARTESIAN_POINT('Ctrl Pts',(1.34824783112887,1.,-1.73425417885907));
#31040=CARTESIAN_POINT('Ctrl Pts',(1.34854391898045,-1.,-1.73682580585691));
#31041=CARTESIAN_POINT('Ctrl Pts',(1.34854391898045,1.,-1.73682580585691));
#31042=CARTESIAN_POINT('Ctrl Pts',(1.34869019493419,-1.,-1.73811241238545));
#31043=CARTESIAN_POINT('Ctrl Pts',(1.34869019493419,1.,-1.73811241238545));
#31044=CARTESIAN_POINT('',(1.15624053661742,1.,-1.31362392696032));
#31045=CARTESIAN_POINT('Ctrl Pts',(1.15624053661742,1.,-1.31362392696032));
#31046=CARTESIAN_POINT('Ctrl Pts',(1.15950888730809,1.,-1.31722977216397));
#31047=CARTESIAN_POINT('Ctrl Pts',(1.16589330093588,1.,-1.32428080721772));
#31048=CARTESIAN_POINT('Ctrl Pts',(1.17501305789857,1.,-1.33437539347008));
#31049=CARTESIAN_POINT('Ctrl Pts',(1.18625865667441,1.,-1.34687054001093));
#31050=CARTESIAN_POINT('Ctrl Pts',(1.1987959077932,1.,-1.36088705043885));
#31051=CARTESIAN_POINT('Ctrl Pts',(1.20982812925645,1.,-1.37331915607905));
#31052=CARTESIAN_POINT('Ctrl Pts',(1.21938737280852,1.,-1.38420564527715));
#31053=CARTESIAN_POINT('Ctrl Pts',(1.22752961899387,1.,-1.39361389568796));
#31054=CARTESIAN_POINT('Ctrl Pts',(1.23434087290423,1.,-1.40164708206106));
#31055=CARTESIAN_POINT('Ctrl Pts',(1.23994455029534,1.,-1.40845295531283));
#31056=CARTESIAN_POINT('Ctrl Pts',(1.24450600513056,1.,-1.41422913175179));
#31057=CARTESIAN_POINT('Ctrl Pts',(1.24824430986571,1.,-1.41923722596025));
#31058=CARTESIAN_POINT('Ctrl Pts',(1.2514145557001,1.,-1.42378102115575));
#31059=CARTESIAN_POINT('Ctrl Pts',(1.25426945222639,1.,-1.42815938799387));
#31060=CARTESIAN_POINT('Ctrl Pts',(1.25702687965755,1.,-1.43262645609691));
#31061=CARTESIAN_POINT('Ctrl Pts',(1.25983531012005,1.,-1.43734919180848));
#31062=CARTESIAN_POINT('Ctrl Pts',(1.26273903323858,1.,-1.44236470511303));
#31063=CARTESIAN_POINT('Ctrl Pts',(1.26570925118868,1.,-1.44761985001662));
#31064=CARTESIAN_POINT('Ctrl Pts',(1.2686778680489,1.,-1.45301422764247));
#31065=CARTESIAN_POINT('Ctrl Pts',(1.27156805265289,1.,-1.45843906294697));
#31066=CARTESIAN_POINT('Ctrl Pts',(1.27433119897822,1.,-1.46382431332476));
#31067=CARTESIAN_POINT('Ctrl Pts',(1.27696414831089,1.,-1.46916035917133));
#31068=CARTESIAN_POINT('Ctrl Pts',(1.2794891824849,1.,-1.4744717526707));
#31069=CARTESIAN_POINT('Ctrl Pts',(1.28194158939517,1.,-1.47980070347096));
#31070=CARTESIAN_POINT('Ctrl Pts',(1.28435533880201,1.,-1.4851881711891));
#31071=CARTESIAN_POINT('Ctrl Pts',(1.2867467611644,1.,-1.4906522831278));
#31072=CARTESIAN_POINT('Ctrl Pts',(1.28911506584254,1.,-1.49618896881754));
#31073=CARTESIAN_POINT('Ctrl Pts',(1.29145022885181,1.,-1.50178230149776));
#31074=CARTESIAN_POINT('Ctrl Pts',(1.29373841372842,1.,-1.50741159078365));
#31075=CARTESIAN_POINT('Ctrl Pts',(1.29596850710509,1.,-1.51305994241402));
#31076=CARTESIAN_POINT('Ctrl Pts',(1.29813791800747,1.,-1.51872184912724));
#31077=CARTESIAN_POINT('Ctrl Pts',(1.30024984366328,1.,-1.52439957861062));
#31078=CARTESIAN_POINT('Ctrl Pts',(1.30231064395568,1.,-1.53009970283891));
#31079=CARTESIAN_POINT('Ctrl Pts',(1.30432735639489,1.,-1.53582981268977));
#31080=CARTESIAN_POINT('Ctrl Pts',(1.30630475189556,1.,-1.54159462645432));
#31081=CARTESIAN_POINT('Ctrl Pts',(1.30824393907473,1.,-1.54739413957185));
#31082=CARTESIAN_POINT('Ctrl Pts',(1.31014393684222,1.,-1.55322568759481));
#31083=CARTESIAN_POINT('Ctrl Pts',(1.31200264341696,1.,-1.55908521254821));
#31084=CARTESIAN_POINT('Ctrl Pts',(1.31381795281002,1.,-1.56496872402353));
#31085=CARTESIAN_POINT('Ctrl Pts',(1.31558903860016,1.,-1.57087397835723));
#31086=CARTESIAN_POINT('Ctrl Pts',(1.31731642317187,1.,-1.5768005650559));
#31087=CARTESIAN_POINT('Ctrl Pts',(1.31900135021432,1.,-1.58274907898834));
#31088=CARTESIAN_POINT('Ctrl Pts',(1.32064537110892,1.,-1.58872057258245));
#31089=CARTESIAN_POINT('Ctrl Pts',(1.32224985747682,1.,-1.59471591079403));
#31090=CARTESIAN_POINT('Ctrl Pts',(1.32381550858256,1.,-1.60073511858687));
#31091=CARTESIAN_POINT('Ctrl Pts',(1.32534250785782,1.,-1.60677758290954));
#31092=CARTESIAN_POINT('Ctrl Pts',(1.32683074483356,1.,-1.6128423401575));
#31093=CARTESIAN_POINT('Ctrl Pts',(1.32828000610449,1.,-1.61892832270724));
#31094=CARTESIAN_POINT('Ctrl Pts',(1.3296901950568,1.,-1.62503464209797));
#31095=CARTESIAN_POINT('Ctrl Pts',(1.33106149345645,1.,-1.63116079730923));
#31096=CARTESIAN_POINT('Ctrl Pts',(1.33239425103724,1.,-1.63730653475089));
#31097=CARTESIAN_POINT('Ctrl Pts',(1.33368890676572,1.,-1.6434717485603));
#31098=CARTESIAN_POINT('Ctrl Pts',(1.33494590467993,1.,-1.6496563728683));
#31099=CARTESIAN_POINT('Ctrl Pts',(1.33616559745172,1.,-1.65586025952593));
#31100=CARTESIAN_POINT('Ctrl Pts',(1.33734820885262,1.,-1.66208312541983));
#31101=CARTESIAN_POINT('Ctrl Pts',(1.33849388654388,1.,-1.66832460783989));
#31102=CARTESIAN_POINT('Ctrl Pts',(1.3396027347034,1.,-1.67458429426086));
#31103=CARTESIAN_POINT('Ctrl Pts',(1.34067485185203,1.,-1.68086176030362));
#31104=CARTESIAN_POINT('Ctrl Pts',(1.341710374848,1.,-1.68715660868764));
#31105=CARTESIAN_POINT('Ctrl Pts',(1.34270948206319,1.,-1.6934684849687));
#31106=CARTESIAN_POINT('Ctrl Pts',(1.34367237124483,1.,-1.69979707754427));
#31107=CARTESIAN_POINT('Ctrl Pts',(1.34459924533831,1.,-1.70614212266738));
#31108=CARTESIAN_POINT('Ctrl Pts',(1.34549029589416,1.,-1.71250340686822));
#31109=CARTESIAN_POINT('Ctrl Pts',(1.34634568653227,1.,-1.7188807715049));
#31110=CARTESIAN_POINT('Ctrl Pts',(1.34716554819527,1.,-1.72527410680674));
#31111=CARTESIAN_POINT('Ctrl Pts',(1.34779309152035,1.,-1.7304014965394));
#31112=CARTESIAN_POINT('Ctrl Pts',(1.34824783112887,1.,-1.73425417885907));
#31113=CARTESIAN_POINT('Ctrl Pts',(1.34854391898045,1.,-1.73682580585691));
#31114=CARTESIAN_POINT('Ctrl Pts',(1.34869019493419,1.,-1.73811241238545));
#31115=CARTESIAN_POINT('',(1.15624053661742,0.,-1.31362392696032));
#31116=CARTESIAN_POINT('Origin',(0.,0.,0.));
#31117=CARTESIAN_POINT('',(1.31362392696032,1.,-1.15624053661742));
#31118=CARTESIAN_POINT('Origin',(0.,1.,0.));
#31119=CARTESIAN_POINT('',(1.31362392696032,0.,-1.15624053661742));
#31120=CARTESIAN_POINT('Ctrl Pts',(1.73811241238545,-1.,-1.34869019493419));
#31121=CARTESIAN_POINT('Ctrl Pts',(1.73811241238545,1.,-1.34869019493419));
#31122=CARTESIAN_POINT('Ctrl Pts',(1.73682580585819,-1.,-1.34854391898145));
#31123=CARTESIAN_POINT('Ctrl Pts',(1.73682580585819,1.,-1.34854391898145));
#31124=CARTESIAN_POINT('Ctrl Pts',(1.73425417886254,-1.,-1.34824783113158));
#31125=CARTESIAN_POINT('Ctrl Pts',(1.73425417886254,1.,-1.34824783113158));
#31126=CARTESIAN_POINT('Ctrl Pts',(1.73040149654497,-1.,-1.3477930915247));
#31127=CARTESIAN_POINT('Ctrl Pts',(1.73040149654497,1.,-1.3477930915247));
#31128=CARTESIAN_POINT('Ctrl Pts',(1.72527410681298,-1.,-1.34716554820013));
#31129=CARTESIAN_POINT('Ctrl Pts',(1.72527410681298,1.,-1.34716554820013));
#31130=CARTESIAN_POINT('Ctrl Pts',(1.7188807715095,-1.,-1.34634568653586));
#31131=CARTESIAN_POINT('Ctrl Pts',(1.7188807715095,1.,-1.34634568653586));
#31132=CARTESIAN_POINT('Ctrl Pts',(1.71250340687011,-1.,-1.34549029589563));
#31133=CARTESIAN_POINT('Ctrl Pts',(1.71250340687011,1.,-1.34549029589563));
#31134=CARTESIAN_POINT('Ctrl Pts',(1.70614212266676,-1.,-1.34459924533783));
#31135=CARTESIAN_POINT('Ctrl Pts',(1.70614212266676,1.,-1.34459924533783));
#31136=CARTESIAN_POINT('Ctrl Pts',(1.69979707754221,-1.,-1.34367237124322));
#31137=CARTESIAN_POINT('Ctrl Pts',(1.69979707754221,1.,-1.34367237124322));
#31138=CARTESIAN_POINT('Ctrl Pts',(1.6934684849664,-1.,-1.34270948206139));
#31139=CARTESIAN_POINT('Ctrl Pts',(1.6934684849664,1.,-1.34270948206139));
#31140=CARTESIAN_POINT('Ctrl Pts',(1.68715660868602,-1.,-1.34171037484673));
#31141=CARTESIAN_POINT('Ctrl Pts',(1.68715660868602,1.,-1.34171037484673));
#31142=CARTESIAN_POINT('Ctrl Pts',(1.68086176030308,-1.,-1.3406748518516));
#31143=CARTESIAN_POINT('Ctrl Pts',(1.68086176030308,1.,-1.3406748518516));
#31144=CARTESIAN_POINT('Ctrl Pts',(1.67458429426126,-1.,-1.33960273470372));
#31145=CARTESIAN_POINT('Ctrl Pts',(1.67458429426126,1.,-1.33960273470372));
#31146=CARTESIAN_POINT('Ctrl Pts',(1.66832460784078,-1.,-1.33849388654458));
#31147=CARTESIAN_POINT('Ctrl Pts',(1.66832460784078,1.,-1.33849388654458));
#31148=CARTESIAN_POINT('Ctrl Pts',(1.66208312542073,-1.,-1.33734820885331));
#31149=CARTESIAN_POINT('Ctrl Pts',(1.66208312542073,1.,-1.33734820885331));
#31150=CARTESIAN_POINT('Ctrl Pts',(1.65586025952651,-1.,-1.33616559745217));
#31151=CARTESIAN_POINT('Ctrl Pts',(1.65586025952651,1.,-1.33616559745217));
#31152=CARTESIAN_POINT('Ctrl Pts',(1.64965637286843,-1.,-1.33494590468003));
#31153=CARTESIAN_POINT('Ctrl Pts',(1.64965637286843,1.,-1.33494590468003));
#31154=CARTESIAN_POINT('Ctrl Pts',(1.64347174856007,-1.,-1.33368890676554));
#31155=CARTESIAN_POINT('Ctrl Pts',(1.64347174856007,1.,-1.33368890676554));
#31156=CARTESIAN_POINT('Ctrl Pts',(1.63730653475049,-1.,-1.33239425103694));
#31157=CARTESIAN_POINT('Ctrl Pts',(1.63730653475049,1.,-1.33239425103694));
#31158=CARTESIAN_POINT('Ctrl Pts',(1.63116079730887,-1.,-1.33106149345618));
#31159=CARTESIAN_POINT('Ctrl Pts',(1.63116079730887,1.,-1.33106149345618));
#31160=CARTESIAN_POINT('Ctrl Pts',(1.62503464209777,-1.,-1.32969019505665));
#31161=CARTESIAN_POINT('Ctrl Pts',(1.62503464209777,1.,-1.32969019505665));
#31162=CARTESIAN_POINT('Ctrl Pts',(1.61892832270723,-1.,-1.32828000610448));
#31163=CARTESIAN_POINT('Ctrl Pts',(1.61892832270723,1.,-1.32828000610448));
#31164=CARTESIAN_POINT('Ctrl Pts',(1.61284234015762,-1.,-1.32683074483365));
#31165=CARTESIAN_POINT('Ctrl Pts',(1.61284234015762,1.,-1.32683074483365));
#31166=CARTESIAN_POINT('Ctrl Pts',(1.6067775829097,-1.,-1.32534250785794));
#31167=CARTESIAN_POINT('Ctrl Pts',(1.6067775829097,1.,-1.32534250785794));
#31168=CARTESIAN_POINT('Ctrl Pts',(1.600735118587,-1.,-1.32381550858266));
#31169=CARTESIAN_POINT('Ctrl Pts',(1.600735118587,1.,-1.32381550858266));
#31170=CARTESIAN_POINT('Ctrl Pts',(1.59471591079408,-1.,-1.32224985747686));
#31171=CARTESIAN_POINT('Ctrl Pts',(1.59471591079408,1.,-1.32224985747686));
#31172=CARTESIAN_POINT('Ctrl Pts',(1.58872057258244,-1.,-1.32064537110891));
#31173=CARTESIAN_POINT('Ctrl Pts',(1.58872057258244,1.,-1.32064537110891));
#31174=CARTESIAN_POINT('Ctrl Pts',(1.58274907898829,-1.,-1.31900135021428));
#31175=CARTESIAN_POINT('Ctrl Pts',(1.58274907898829,1.,-1.31900135021428));
#31176=CARTESIAN_POINT('Ctrl Pts',(1.57680056505585,-1.,-1.31731642317183));
#31177=CARTESIAN_POINT('Ctrl Pts',(1.57680056505585,1.,-1.31731642317183));
#31178=CARTESIAN_POINT('Ctrl Pts',(1.57087397835721,-1.,-1.31558903860015));
#31179=CARTESIAN_POINT('Ctrl Pts',(1.57087397835721,1.,-1.31558903860015));
#31180=CARTESIAN_POINT('Ctrl Pts',(1.56496872402352,-1.,-1.31381795281002));
#31181=CARTESIAN_POINT('Ctrl Pts',(1.56496872402352,1.,-1.31381795281002));
#31182=CARTESIAN_POINT('Ctrl Pts',(1.55908521254822,-1.,-1.31200264341696));
#31183=CARTESIAN_POINT('Ctrl Pts',(1.55908521254822,1.,-1.31200264341696));
#31184=CARTESIAN_POINT('Ctrl Pts',(1.55322568759481,-1.,-1.31014393684221));
#31185=CARTESIAN_POINT('Ctrl Pts',(1.55322568759481,1.,-1.31014393684221));
#31186=CARTESIAN_POINT('Ctrl Pts',(1.54739413957183,-1.,-1.30824393907471));
#31187=CARTESIAN_POINT('Ctrl Pts',(1.54739413957183,1.,-1.30824393907471));
#31188=CARTESIAN_POINT('Ctrl Pts',(1.54159462645428,-1.,-1.30630475189553));
#31189=CARTESIAN_POINT('Ctrl Pts',(1.54159462645428,1.,-1.30630475189553));
#31190=CARTESIAN_POINT('Ctrl Pts',(1.53582981268976,-1.,-1.30432735639487));
#31191=CARTESIAN_POINT('Ctrl Pts',(1.53582981268976,1.,-1.30432735639487));
#31192=CARTESIAN_POINT('Ctrl Pts',(1.53009970283893,-1.,-1.3023106439557));
#31193=CARTESIAN_POINT('Ctrl Pts',(1.53009970283893,1.,-1.3023106439557));
#31194=CARTESIAN_POINT('Ctrl Pts',(1.5243995786107,-1.,-1.30024984366334));
#31195=CARTESIAN_POINT('Ctrl Pts',(1.5243995786107,1.,-1.30024984366334));
#31196=CARTESIAN_POINT('Ctrl Pts',(1.51872184912735,-1.,-1.29813791800757));
#31197=CARTESIAN_POINT('Ctrl Pts',(1.51872184912735,1.,-1.29813791800757));
#31198=CARTESIAN_POINT('Ctrl Pts',(1.51305994241412,-1.,-1.29596850710518));
#31199=CARTESIAN_POINT('Ctrl Pts',(1.51305994241412,1.,-1.29596850710518));
#31200=CARTESIAN_POINT('Ctrl Pts',(1.50741159078367,-1.,-1.29373841372843));
#31201=CARTESIAN_POINT('Ctrl Pts',(1.50741159078367,1.,-1.29373841372843));
#31202=CARTESIAN_POINT('Ctrl Pts',(1.50178230149764,-1.,-1.29145022885171));
#31203=CARTESIAN_POINT('Ctrl Pts',(1.50178230149764,1.,-1.29145022885171));
#31204=CARTESIAN_POINT('Ctrl Pts',(1.49618896881729,-1.,-1.28911506584232));
#31205=CARTESIAN_POINT('Ctrl Pts',(1.49618896881729,1.,-1.28911506584232));
#31206=CARTESIAN_POINT('Ctrl Pts',(1.4906522831275,-1.,-1.28674676116415));
#31207=CARTESIAN_POINT('Ctrl Pts',(1.4906522831275,1.,-1.28674676116415));
#31208=CARTESIAN_POINT('Ctrl Pts',(1.48518817118891,-1.,-1.28435533880184));
#31209=CARTESIAN_POINT('Ctrl Pts',(1.48518817118891,1.,-1.28435533880184));
#31210=CARTESIAN_POINT('Ctrl Pts',(1.47980070347102,-1.,-1.28194158939522));
#31211=CARTESIAN_POINT('Ctrl Pts',(1.47980070347102,1.,-1.28194158939522));
#31212=CARTESIAN_POINT('Ctrl Pts',(1.4744717526711,-1.,-1.27948918248524));
#31213=CARTESIAN_POINT('Ctrl Pts',(1.4744717526711,1.,-1.27948918248524));
#31214=CARTESIAN_POINT('Ctrl Pts',(1.46916035917197,-1.,-1.27696414831144));
#31215=CARTESIAN_POINT('Ctrl Pts',(1.46916035917197,1.,-1.27696414831144));
#31216=CARTESIAN_POINT('Ctrl Pts',(1.4638243133254,-1.,-1.27433119897877));
#31217=CARTESIAN_POINT('Ctrl Pts',(1.4638243133254,1.,-1.27433119897877));
#31218=CARTESIAN_POINT('Ctrl Pts',(1.45843906294725,-1.,-1.27156805265312));
#31219=CARTESIAN_POINT('Ctrl Pts',(1.45843906294725,1.,-1.27156805265312));
#31220=CARTESIAN_POINT('Ctrl Pts',(1.45301422764205,-1.,-1.26867786804854));
#31221=CARTESIAN_POINT('Ctrl Pts',(1.45301422764205,1.,-1.26867786804854));
#31222=CARTESIAN_POINT('Ctrl Pts',(1.44761985001544,-1.,-1.26570925118767));
#31223=CARTESIAN_POINT('Ctrl Pts',(1.44761985001544,1.,-1.26570925118767));
#31224=CARTESIAN_POINT('Ctrl Pts',(1.44236470511145,-1.,-1.26273903323723));
#31225=CARTESIAN_POINT('Ctrl Pts',(1.44236470511145,1.,-1.26273903323723));
#31226=CARTESIAN_POINT('Ctrl Pts',(1.43734919180719,-1.,-1.25983531011894));
#31227=CARTESIAN_POINT('Ctrl Pts',(1.43734919180719,1.,-1.25983531011894));
#31228=CARTESIAN_POINT('Ctrl Pts',(1.43262645609679,-1.,-1.25702687965744));
#31229=CARTESIAN_POINT('Ctrl Pts',(1.43262645609679,1.,-1.25702687965744));
#31230=CARTESIAN_POINT('Ctrl Pts',(1.42815938799555,-1.,-1.25426945222783));
#31231=CARTESIAN_POINT('Ctrl Pts',(1.42815938799555,1.,-1.25426945222783));
#31232=CARTESIAN_POINT('Ctrl Pts',(1.42378102115911,-1.,-1.25141455570299));
#31233=CARTESIAN_POINT('Ctrl Pts',(1.42378102115911,1.,-1.25141455570299));
#31234=CARTESIAN_POINT('Ctrl Pts',(1.41923722596421,-1.,-1.24824430986911));
#31235=CARTESIAN_POINT('Ctrl Pts',(1.41923722596421,1.,-1.24824430986911));
#31236=CARTESIAN_POINT('Ctrl Pts',(1.41422913175437,-1.,-1.24450600513278));
#31237=CARTESIAN_POINT('Ctrl Pts',(1.41422913175437,1.,-1.24450600513278));
#31238=CARTESIAN_POINT('Ctrl Pts',(1.40845295531151,-1.,-1.23994455029421));
#31239=CARTESIAN_POINT('Ctrl Pts',(1.40845295531151,1.,-1.23994455029421));
#31240=CARTESIAN_POINT('Ctrl Pts',(1.40164708205345,-1.,-1.23434087289768));
#31241=CARTESIAN_POINT('Ctrl Pts',(1.40164708205345,1.,-1.23434087289768));
#31242=CARTESIAN_POINT('Ctrl Pts',(1.39361389567257,-1.,-1.22752961898063));
#31243=CARTESIAN_POINT('Ctrl Pts',(1.39361389567257,1.,-1.22752961898063));
#31244=CARTESIAN_POINT('Ctrl Pts',(1.38420564525391,-1.,-1.21938737278853));
#31245=CARTESIAN_POINT('Ctrl Pts',(1.38420564525391,1.,-1.21938737278853));
#31246=CARTESIAN_POINT('Ctrl Pts',(1.37331915604962,-1.,-1.20982812923113));
#31247=CARTESIAN_POINT('Ctrl Pts',(1.37331915604962,1.,-1.20982812923113));
#31248=CARTESIAN_POINT('Ctrl Pts',(1.36088705040677,-1.,-1.1987959077656));
#31249=CARTESIAN_POINT('Ctrl Pts',(1.36088705040677,1.,-1.1987959077656));
#31250=CARTESIAN_POINT('Ctrl Pts',(1.34687053998157,-1.,-1.18625865664915));
#31251=CARTESIAN_POINT('Ctrl Pts',(1.34687053998157,1.,-1.18625865664915));
#31252=CARTESIAN_POINT('Ctrl Pts',(1.33437539344842,-1.,-1.17501305787994));
#31253=CARTESIAN_POINT('Ctrl Pts',(1.33437539344842,1.,-1.17501305787994));
#31254=CARTESIAN_POINT('Ctrl Pts',(1.32428080720544,-1.,-1.16589330092532));
#31255=CARTESIAN_POINT('Ctrl Pts',(1.32428080720544,1.,-1.16589330092532));
#31256=CARTESIAN_POINT('Ctrl Pts',(1.3172297721596,-1.,-1.15950888730433));
#31257=CARTESIAN_POINT('Ctrl Pts',(1.3172297721596,1.,-1.15950888730433));
#31258=CARTESIAN_POINT('Ctrl Pts',(1.31362392696032,-1.,-1.15624053661742));
#31259=CARTESIAN_POINT('Ctrl Pts',(1.31362392696032,1.,-1.15624053661742));
#31260=CARTESIAN_POINT('',(1.73811241238545,1.,-1.34869019493419));
#31261=CARTESIAN_POINT('Ctrl Pts',(1.73811241238545,1.,-1.34869019493419));
#31262=CARTESIAN_POINT('Ctrl Pts',(1.73682580585819,1.,-1.34854391898145));
#31263=CARTESIAN_POINT('Ctrl Pts',(1.73425417886254,1.,-1.34824783113158));
#31264=CARTESIAN_POINT('Ctrl Pts',(1.73040149654497,1.,-1.3477930915247));
#31265=CARTESIAN_POINT('Ctrl Pts',(1.72527410681298,1.,-1.34716554820013));
#31266=CARTESIAN_POINT('Ctrl Pts',(1.7188807715095,1.,-1.34634568653586));
#31267=CARTESIAN_POINT('Ctrl Pts',(1.71250340687011,1.,-1.34549029589563));
#31268=CARTESIAN_POINT('Ctrl Pts',(1.70614212266676,1.,-1.34459924533783));
#31269=CARTESIAN_POINT('Ctrl Pts',(1.69979707754221,1.,-1.34367237124322));
#31270=CARTESIAN_POINT('Ctrl Pts',(1.6934684849664,1.,-1.34270948206139));
#31271=CARTESIAN_POINT('Ctrl Pts',(1.68715660868602,1.,-1.34171037484673));
#31272=CARTESIAN_POINT('Ctrl Pts',(1.68086176030308,1.,-1.3406748518516));
#31273=CARTESIAN_POINT('Ctrl Pts',(1.67458429426126,1.,-1.33960273470372));
#31274=CARTESIAN_POINT('Ctrl Pts',(1.66832460784078,1.,-1.33849388654458));
#31275=CARTESIAN_POINT('Ctrl Pts',(1.66208312542073,1.,-1.33734820885331));
#31276=CARTESIAN_POINT('Ctrl Pts',(1.65586025952651,1.,-1.33616559745217));
#31277=CARTESIAN_POINT('Ctrl Pts',(1.64965637286843,1.,-1.33494590468003));
#31278=CARTESIAN_POINT('Ctrl Pts',(1.64347174856007,1.,-1.33368890676554));
#31279=CARTESIAN_POINT('Ctrl Pts',(1.63730653475049,1.,-1.33239425103694));
#31280=CARTESIAN_POINT('Ctrl Pts',(1.63116079730887,1.,-1.33106149345618));
#31281=CARTESIAN_POINT('Ctrl Pts',(1.62503464209777,1.,-1.32969019505665));
#31282=CARTESIAN_POINT('Ctrl Pts',(1.61892832270723,1.,-1.32828000610448));
#31283=CARTESIAN_POINT('Ctrl Pts',(1.61284234015762,1.,-1.32683074483365));
#31284=CARTESIAN_POINT('Ctrl Pts',(1.6067775829097,1.,-1.32534250785794));
#31285=CARTESIAN_POINT('Ctrl Pts',(1.600735118587,1.,-1.32381550858266));
#31286=CARTESIAN_POINT('Ctrl Pts',(1.59471591079408,1.,-1.32224985747686));
#31287=CARTESIAN_POINT('Ctrl Pts',(1.58872057258244,1.,-1.32064537110891));
#31288=CARTESIAN_POINT('Ctrl Pts',(1.58274907898829,1.,-1.31900135021428));
#31289=CARTESIAN_POINT('Ctrl Pts',(1.57680056505585,1.,-1.31731642317183));
#31290=CARTESIAN_POINT('Ctrl Pts',(1.57087397835721,1.,-1.31558903860015));
#31291=CARTESIAN_POINT('Ctrl Pts',(1.56496872402352,1.,-1.31381795281002));
#31292=CARTESIAN_POINT('Ctrl Pts',(1.55908521254822,1.,-1.31200264341696));
#31293=CARTESIAN_POINT('Ctrl Pts',(1.55322568759481,1.,-1.31014393684221));
#31294=CARTESIAN_POINT('Ctrl Pts',(1.54739413957183,1.,-1.30824393907471));
#31295=CARTESIAN_POINT('Ctrl Pts',(1.54159462645428,1.,-1.30630475189553));
#31296=CARTESIAN_POINT('Ctrl Pts',(1.53582981268976,1.,-1.30432735639487));
#31297=CARTESIAN_POINT('Ctrl Pts',(1.53009970283893,1.,-1.3023106439557));
#31298=CARTESIAN_POINT('Ctrl Pts',(1.5243995786107,1.,-1.30024984366334));
#31299=CARTESIAN_POINT('Ctrl Pts',(1.51872184912735,1.,-1.29813791800757));
#31300=CARTESIAN_POINT('Ctrl Pts',(1.51305994241412,1.,-1.29596850710518));
#31301=CARTESIAN_POINT('Ctrl Pts',(1.50741159078367,1.,-1.29373841372843));
#31302=CARTESIAN_POINT('Ctrl Pts',(1.50178230149764,1.,-1.29145022885171));
#31303=CARTESIAN_POINT('Ctrl Pts',(1.49618896881729,1.,-1.28911506584232));
#31304=CARTESIAN_POINT('Ctrl Pts',(1.4906522831275,1.,-1.28674676116415));
#31305=CARTESIAN_POINT('Ctrl Pts',(1.48518817118891,1.,-1.28435533880184));
#31306=CARTESIAN_POINT('Ctrl Pts',(1.47980070347102,1.,-1.28194158939522));
#31307=CARTESIAN_POINT('Ctrl Pts',(1.4744717526711,1.,-1.27948918248524));
#31308=CARTESIAN_POINT('Ctrl Pts',(1.46916035917197,1.,-1.27696414831144));
#31309=CARTESIAN_POINT('Ctrl Pts',(1.4638243133254,1.,-1.27433119897877));
#31310=CARTESIAN_POINT('Ctrl Pts',(1.45843906294725,1.,-1.27156805265312));
#31311=CARTESIAN_POINT('Ctrl Pts',(1.45301422764205,1.,-1.26867786804854));
#31312=CARTESIAN_POINT('Ctrl Pts',(1.44761985001544,1.,-1.26570925118767));
#31313=CARTESIAN_POINT('Ctrl Pts',(1.44236470511145,1.,-1.26273903323723));
#31314=CARTESIAN_POINT('Ctrl Pts',(1.43734919180719,1.,-1.25983531011894));
#31315=CARTESIAN_POINT('Ctrl Pts',(1.43262645609679,1.,-1.25702687965744));
#31316=CARTESIAN_POINT('Ctrl Pts',(1.42815938799555,1.,-1.25426945222783));
#31317=CARTESIAN_POINT('Ctrl Pts',(1.42378102115911,1.,-1.25141455570299));
#31318=CARTESIAN_POINT('Ctrl Pts',(1.41923722596421,1.,-1.24824430986911));
#31319=CARTESIAN_POINT('Ctrl Pts',(1.41422913175437,1.,-1.24450600513278));
#31320=CARTESIAN_POINT('Ctrl Pts',(1.40845295531151,1.,-1.23994455029421));
#31321=CARTESIAN_POINT('Ctrl Pts',(1.40164708205345,1.,-1.23434087289768));
#31322=CARTESIAN_POINT('Ctrl Pts',(1.39361389567257,1.,-1.22752961898063));
#31323=CARTESIAN_POINT('Ctrl Pts',(1.38420564525391,1.,-1.21938737278853));
#31324=CARTESIAN_POINT('Ctrl Pts',(1.37331915604962,1.,-1.20982812923113));
#31325=CARTESIAN_POINT('Ctrl Pts',(1.36088705040677,1.,-1.1987959077656));
#31326=CARTESIAN_POINT('Ctrl Pts',(1.34687053998157,1.,-1.18625865664915));
#31327=CARTESIAN_POINT('Ctrl Pts',(1.33437539344842,1.,-1.17501305787994));
#31328=CARTESIAN_POINT('Ctrl Pts',(1.32428080720544,1.,-1.16589330092532));
#31329=CARTESIAN_POINT('Ctrl Pts',(1.3172297721596,1.,-1.15950888730433));
#31330=CARTESIAN_POINT('Ctrl Pts',(1.31362392696032,1.,-1.15624053661742));
#31331=CARTESIAN_POINT('',(1.73811241238545,0.,-1.34869019493419));
#31332=CARTESIAN_POINT('Origin',(1.81978687191668,0.,-1.23627494547115));
#31333=CARTESIAN_POINT('',(1.81978687191668,1.,-1.23627494547115));
#31334=CARTESIAN_POINT('',(1.73811241238545,1.,-1.34869019493419));
#31335=CARTESIAN_POINT('',(1.81978687191668,0.,-1.23627494547115));
#31336=CARTESIAN_POINT('Ctrl Pts',(1.5055822144029,-1.,-0.892032620296855));
#31337=CARTESIAN_POINT('Ctrl Pts',(1.5055822144029,1.,-0.892032620296855));
#31338=CARTESIAN_POINT('Ctrl Pts',(1.50980486807181,-1.,-0.894452006967538));
#31339=CARTESIAN_POINT('Ctrl Pts',(1.50980486807181,1.,-0.894452006967538));
#31340=CARTESIAN_POINT('Ctrl Pts',(1.51805569591479,-1.,-0.89918504749193));
#31341=CARTESIAN_POINT('Ctrl Pts',(1.51805569591479,1.,-0.89918504749193));
#31342=CARTESIAN_POINT('Ctrl Pts',(1.52984849890434,-1.,-0.905967409640499));
#31343=CARTESIAN_POINT('Ctrl Pts',(1.52984849890434,1.,-0.905967409640499));
#31344=CARTESIAN_POINT('Ctrl Pts',(1.54440491152807,-1.,-0.91437591904658));
#31345=CARTESIAN_POINT('Ctrl Pts',(1.54440491152807,1.,-0.91437591904658));
#31346=CARTESIAN_POINT('Ctrl Pts',(1.56065988582509,-1.,-0.923832188966322));
#31347=CARTESIAN_POINT('Ctrl Pts',(1.56065988582509,1.,-0.923832188966322));
#31348=CARTESIAN_POINT('Ctrl Pts',(1.57499388385561,-1.,-0.932246680128849));
#31349=CARTESIAN_POINT('Ctrl Pts',(1.57499388385561,1.,-0.932246680128849));
#31350=CARTESIAN_POINT('Ctrl Pts',(1.58744937489796,-1.,-0.939646377909319));
#31351=CARTESIAN_POINT('Ctrl Pts',(1.58744937489796,1.,-0.939646377909319));
#31352=CARTESIAN_POINT('Ctrl Pts',(1.59810042045408,-1.,-0.946078063325796));
#31353=CARTESIAN_POINT('Ctrl Pts',(1.59810042045408,1.,-0.946078063325796));
#31354=CARTESIAN_POINT('Ctrl Pts',(1.60706069897794,-1.,-0.951613284361248));
#31355=CARTESIAN_POINT('Ctrl Pts',(1.60706069897794,1.,-0.951613284361248));
#31356=CARTESIAN_POINT('Ctrl Pts',(1.61449324337233,-1.,-0.956354422921573));
#31357=CARTESIAN_POINT('Ctrl Pts',(1.61449324337233,1.,-0.956354422921573));
#31358=CARTESIAN_POINT('Ctrl Pts',(1.62061638139929,-1.,-0.960438326099958));
#31359=CARTESIAN_POINT('Ctrl Pts',(1.62061638139929,1.,-0.960438326099958));
#31360=CARTESIAN_POINT('Ctrl Pts',(1.6257193066974,-1.,-0.964046107037821));
#31361=CARTESIAN_POINT('Ctrl Pts',(1.6257193066974,1.,-0.964046107037821));
#31362=CARTESIAN_POINT('Ctrl Pts',(1.63013849959083,-1.,-0.967387853228041));
#31363=CARTESIAN_POINT('Ctrl Pts',(1.63013849959083,1.,-0.967387853228041));
#31364=CARTESIAN_POINT('Ctrl Pts',(1.63420665729609,-1.,-0.970669715996356));
#31365=CARTESIAN_POINT('Ctrl Pts',(1.63420665729609,1.,-0.970669715996356));
#31366=CARTESIAN_POINT('Ctrl Pts',(1.63820952658157,-1.,-0.974066058287501));
#31367=CARTESIAN_POINT('Ctrl Pts',(1.63820952658157,1.,-0.974066058287501));
#31368=CARTESIAN_POINT('Ctrl Pts',(1.64233990826831,-1.,-0.977689794120297));
#31369=CARTESIAN_POINT('Ctrl Pts',(1.64233990826831,1.,-0.977689794120297));
#31370=CARTESIAN_POINT('Ctrl Pts',(1.64665139190834,-1.,-0.981562530940574));
#31371=CARTESIAN_POINT('Ctrl Pts',(1.64665139190834,1.,-0.981562530940574));
#31372=CARTESIAN_POINT('Ctrl Pts',(1.6511001661277,-1.,-0.985642622921626));
#31373=CARTESIAN_POINT('Ctrl Pts',(1.6511001661277,1.,-0.985642622921626));
#31374=CARTESIAN_POINT('Ctrl Pts',(1.65559044289746,-1.,-0.98985562785445));
#31375=CARTESIAN_POINT('Ctrl Pts',(1.65559044289746,1.,-0.98985562785445));
#31376=CARTESIAN_POINT('Ctrl Pts',(1.66001553809916,-1.,-0.994121836661116));
#31377=CARTESIAN_POINT('Ctrl Pts',(1.66001553809916,1.,-0.994121836661116));
#31378=CARTESIAN_POINT('Ctrl Pts',(1.66430758030304,-1.,-0.998389654952317));
#31379=CARTESIAN_POINT('Ctrl Pts',(1.66430758030304,1.,-0.998389654952317));
#31380=CARTESIAN_POINT('Ctrl Pts',(1.66846059277231,-1.,-1.00265091003682));
#31381=CARTESIAN_POINT('Ctrl Pts',(1.66846059277231,1.,-1.00265091003682));
#31382=CARTESIAN_POINT('Ctrl Pts',(1.67250335383248,-1.,-1.00692206696387));
#31383=CARTESIAN_POINT('Ctrl Pts',(1.67250335383248,1.,-1.00692206696387));
#31384=CARTESIAN_POINT('Ctrl Pts',(1.67648246776457,-1.,-1.01123236493507));
#31385=CARTESIAN_POINT('Ctrl Pts',(1.67648246776457,1.,-1.01123236493507));
#31386=CARTESIAN_POINT('Ctrl Pts',(1.6804428989482,-1.,-1.01561026162787));
#31387=CARTESIAN_POINT('Ctrl Pts',(1.6804428989482,1.,-1.01561026162787));
#31388=CARTESIAN_POINT('Ctrl Pts',(1.68440578021739,-1.,-1.02006795074222));
#31389=CARTESIAN_POINT('Ctrl Pts',(1.68440578021739,1.,-1.02006795074222));
#31390=CARTESIAN_POINT('Ctrl Pts',(1.68836910178475,-1.,-1.02460180535272));
#31391=CARTESIAN_POINT('Ctrl Pts',(1.68836910178475,1.,-1.02460180535272));
#31392=CARTESIAN_POINT('Ctrl Pts',(1.69231840863471,-1.,-1.02919977579155));
#31393=CARTESIAN_POINT('Ctrl Pts',(1.69231840863471,1.,-1.02919977579155));
#31394=CARTESIAN_POINT('Ctrl Pts',(1.69623414782769,-1.,-1.03384646003587));
#31395=CARTESIAN_POINT('Ctrl Pts',(1.69623414782769,1.,-1.03384646003587));
#31396=CARTESIAN_POINT('Ctrl Pts',(1.70010052930951,-1.,-1.03852922490782));
#31397=CARTESIAN_POINT('Ctrl Pts',(1.70010052930951,1.,-1.03852922490782));
#31398=CARTESIAN_POINT('Ctrl Pts',(1.70391338707969,-1.,-1.04324363334546));
#31399=CARTESIAN_POINT('Ctrl Pts',(1.70391338707969,1.,-1.04324363334546));
#31400=CARTESIAN_POINT('Ctrl Pts',(1.70767646263641,-1.,-1.0479908540499));
#31401=CARTESIAN_POINT('Ctrl Pts',(1.70767646263641,1.,-1.0479908540499));
#31402=CARTESIAN_POINT('Ctrl Pts',(1.71139783543986,-1.,-1.05277517202854));
#31403=CARTESIAN_POINT('Ctrl Pts',(1.71139783543986,1.,-1.05277517202854));
#31404=CARTESIAN_POINT('Ctrl Pts',(1.71508654427022,-1.,-1.05760163192481));
#31405=CARTESIAN_POINT('Ctrl Pts',(1.71508654427022,1.,-1.05760163192481));
#31406=CARTESIAN_POINT('Ctrl Pts',(1.71874858456908,-1.,-1.0624732468065));
#31407=CARTESIAN_POINT('Ctrl Pts',(1.71874858456908,1.,-1.0624732468065));
#31408=CARTESIAN_POINT('Ctrl Pts',(1.72238500928456,-1.,-1.06738966975463));
#31409=CARTESIAN_POINT('Ctrl Pts',(1.72238500928456,1.,-1.06738966975463));
#31410=CARTESIAN_POINT('Ctrl Pts',(1.72599406198489,-1.,-1.07234866990252));
#31411=CARTESIAN_POINT('Ctrl Pts',(1.72599406198489,1.,-1.07234866990252));
#31412=CARTESIAN_POINT('Ctrl Pts',(1.72957248977424,-1.,-1.0773470373727));
#31413=CARTESIAN_POINT('Ctrl Pts',(1.72957248977424,1.,-1.0773470373727));
#31414=CARTESIAN_POINT('Ctrl Pts',(1.73311705663407,-1.,-1.08238162784749));
#31415=CARTESIAN_POINT('Ctrl Pts',(1.73311705663407,1.,-1.08238162784749));
#31416=CARTESIAN_POINT('Ctrl Pts',(1.73662628326093,-1.,-1.08745056285429));
#31417=CARTESIAN_POINT('Ctrl Pts',(1.73662628326093,1.,-1.08745056285429));
#31418=CARTESIAN_POINT('Ctrl Pts',(1.74010053962252,-1.,-1.09255329056496));
#31419=CARTESIAN_POINT('Ctrl Pts',(1.74010053962252,1.,-1.09255329056496));
#31420=CARTESIAN_POINT('Ctrl Pts',(1.74354119236212,-1.,-1.09768999241229));
#31421=CARTESIAN_POINT('Ctrl Pts',(1.74354119236212,1.,-1.09768999241229));
#31422=CARTESIAN_POINT('Ctrl Pts',(1.74695004214924,-1.,-1.10286118991144));
#31423=CARTESIAN_POINT('Ctrl Pts',(1.74695004214924,1.,-1.10286118991144));
#31424=CARTESIAN_POINT('Ctrl Pts',(1.75032866075914,-1.,-1.10806728183003));
#31425=CARTESIAN_POINT('Ctrl Pts',(1.75032866075914,1.,-1.10806728183003));
#31426=CARTESIAN_POINT('Ctrl Pts',(1.75367772094617,-1.,-1.11330807582542));
#31427=CARTESIAN_POINT('Ctrl Pts',(1.75367772094617,1.,-1.11330807582542));
#31428=CARTESIAN_POINT('Ctrl Pts',(1.75699720772089,-1.,-1.11858293216752));
#31429=CARTESIAN_POINT('Ctrl Pts',(1.75699720772089,1.,-1.11858293216752));
#31430=CARTESIAN_POINT('Ctrl Pts',(1.76028671825084,-1.,-1.12389096855078));
#31431=CARTESIAN_POINT('Ctrl Pts',(1.76028671825084,1.,-1.12389096855078));
#31432=CARTESIAN_POINT('Ctrl Pts',(1.76354571966171,-1.,-1.12923123555076));
#31433=CARTESIAN_POINT('Ctrl Pts',(1.76354571966171,1.,-1.12923123555076));
#31434=CARTESIAN_POINT('Ctrl Pts',(1.76677384551883,-1.,-1.13460291804635));
#31435=CARTESIAN_POINT('Ctrl Pts',(1.76677384551883,1.,-1.13460291804635));
#31436=CARTESIAN_POINT('Ctrl Pts',(1.76997111386806,-1.,-1.14000548337));
#31437=CARTESIAN_POINT('Ctrl Pts',(1.76997111386806,1.,-1.14000548337));
#31438=CARTESIAN_POINT('Ctrl Pts',(1.77313777896234,-1.,-1.14543858226948));
#31439=CARTESIAN_POINT('Ctrl Pts',(1.77313777896234,1.,-1.14543858226948));
#31440=CARTESIAN_POINT('Ctrl Pts',(1.77627422557034,-1.,-1.15090197841531));
#31441=CARTESIAN_POINT('Ctrl Pts',(1.77627422557034,1.,-1.15090197841531));
#31442=CARTESIAN_POINT('Ctrl Pts',(1.77938085564261,-1.,-1.15639547194689));
#31443=CARTESIAN_POINT('Ctrl Pts',(1.77938085564261,1.,-1.15639547194689));
#31444=CARTESIAN_POINT('Ctrl Pts',(1.78245795880949,-1.,-1.16191881298458));
#31445=CARTESIAN_POINT('Ctrl Pts',(1.78245795880949,1.,-1.16191881298458));
#31446=CARTESIAN_POINT('Ctrl Pts',(1.78550566040349,-1.,-1.16747166312239));
#31447=CARTESIAN_POINT('Ctrl Pts',(1.78550566040349,1.,-1.16747166312239));
#31448=CARTESIAN_POINT('Ctrl Pts',(1.78852398877523,-1.,-1.17305363177265));
#31449=CARTESIAN_POINT('Ctrl Pts',(1.78852398877523,1.,-1.17305363177265));
#31450=CARTESIAN_POINT('Ctrl Pts',(1.79151291552646,-1.,-1.17866429440781));
#31451=CARTESIAN_POINT('Ctrl Pts',(1.79151291552646,1.,-1.17866429440781));
#31452=CARTESIAN_POINT('Ctrl Pts',(1.79447240321572,-1.,-1.18430321697471));
#31453=CARTESIAN_POINT('Ctrl Pts',(1.79447240321572,1.,-1.18430321697471));
#31454=CARTESIAN_POINT('Ctrl Pts',(1.79740245923649,-1.,-1.1899699793456));
#31455=CARTESIAN_POINT('Ctrl Pts',(1.79740245923649,1.,-1.1899699793456));
#31456=CARTESIAN_POINT('Ctrl Pts',(1.80030314370121,-1.,-1.19566418930405));
#31457=CARTESIAN_POINT('Ctrl Pts',(1.80030314370121,1.,-1.19566418930405));
#31458=CARTESIAN_POINT('Ctrl Pts',(1.8031745483882,-1.,-1.2013854893912));
#31459=CARTESIAN_POINT('Ctrl Pts',(1.8031745483882,1.,-1.2013854893912));
#31460=CARTESIAN_POINT('Ctrl Pts',(1.80601678480772,-1.,-1.20713356605519));
#31461=CARTESIAN_POINT('Ctrl Pts',(1.80601678480772,1.,-1.20713356605519));
#31462=CARTESIAN_POINT('Ctrl Pts',(1.80882996916931,-1.,-1.2129081570818));
#31463=CARTESIAN_POINT('Ctrl Pts',(1.80882996916931,1.,-1.2129081570818));
#31464=CARTESIAN_POINT('Ctrl Pts',(1.81161420806172,-1.,-1.2187090610323));
#31465=CARTESIAN_POINT('Ctrl Pts',(1.81161420806172,1.,-1.2187090610323));
#31466=CARTESIAN_POINT('Ctrl Pts',(1.81436959209778,-1.,-1.22453613304507));
#31467=CARTESIAN_POINT('Ctrl Pts',(1.81436959209778,1.,-1.22453613304507));
#31468=CARTESIAN_POINT('Ctrl Pts',(1.81655087183054,-1.,-1.22921864890975));
#31469=CARTESIAN_POINT('Ctrl Pts',(1.81655087183054,1.,-1.22921864890975));
#31470=CARTESIAN_POINT('Ctrl Pts',(1.81817389920914,-1.,-1.23274224526804));
#31471=CARTESIAN_POINT('Ctrl Pts',(1.81817389920914,1.,-1.23274224526804));
#31472=CARTESIAN_POINT('Ctrl Pts',(1.81925017193531,-1.,-1.23509651170384));
#31473=CARTESIAN_POINT('Ctrl Pts',(1.81925017193531,1.,-1.23509651170384));
#31474=CARTESIAN_POINT('Ctrl Pts',(1.81978687191668,-1.,-1.23627494547115));
#31475=CARTESIAN_POINT('Ctrl Pts',(1.81978687191668,1.,-1.23627494547115));
#31476=CARTESIAN_POINT('',(1.5055822144029,1.,-0.892032620296855));
#31477=CARTESIAN_POINT('Ctrl Pts',(1.5055822144029,1.,-0.892032620296855));
#31478=CARTESIAN_POINT('Ctrl Pts',(1.50980486807181,1.,-0.894452006967538));
#31479=CARTESIAN_POINT('Ctrl Pts',(1.51805569591479,1.,-0.89918504749193));
#31480=CARTESIAN_POINT('Ctrl Pts',(1.52984849890434,1.,-0.905967409640499));
#31481=CARTESIAN_POINT('Ctrl Pts',(1.54440491152807,1.,-0.91437591904658));
#31482=CARTESIAN_POINT('Ctrl Pts',(1.56065988582509,1.,-0.923832188966322));
#31483=CARTESIAN_POINT('Ctrl Pts',(1.57499388385561,1.,-0.932246680128849));
#31484=CARTESIAN_POINT('Ctrl Pts',(1.58744937489796,1.,-0.939646377909319));
#31485=CARTESIAN_POINT('Ctrl Pts',(1.59810042045408,1.,-0.946078063325796));
#31486=CARTESIAN_POINT('Ctrl Pts',(1.60706069897794,1.,-0.951613284361248));
#31487=CARTESIAN_POINT('Ctrl Pts',(1.61449324337233,1.,-0.956354422921573));
#31488=CARTESIAN_POINT('Ctrl Pts',(1.62061638139929,1.,-0.960438326099958));
#31489=CARTESIAN_POINT('Ctrl Pts',(1.6257193066974,1.,-0.964046107037821));
#31490=CARTESIAN_POINT('Ctrl Pts',(1.63013849959083,1.,-0.967387853228041));
#31491=CARTESIAN_POINT('Ctrl Pts',(1.63420665729609,1.,-0.970669715996356));
#31492=CARTESIAN_POINT('Ctrl Pts',(1.63820952658157,1.,-0.974066058287501));
#31493=CARTESIAN_POINT('Ctrl Pts',(1.64233990826831,1.,-0.977689794120297));
#31494=CARTESIAN_POINT('Ctrl Pts',(1.64665139190834,1.,-0.981562530940574));
#31495=CARTESIAN_POINT('Ctrl Pts',(1.6511001661277,1.,-0.985642622921626));
#31496=CARTESIAN_POINT('Ctrl Pts',(1.65559044289746,1.,-0.98985562785445));
#31497=CARTESIAN_POINT('Ctrl Pts',(1.66001553809916,1.,-0.994121836661116));
#31498=CARTESIAN_POINT('Ctrl Pts',(1.66430758030304,1.,-0.998389654952317));
#31499=CARTESIAN_POINT('Ctrl Pts',(1.66846059277231,1.,-1.00265091003682));
#31500=CARTESIAN_POINT('Ctrl Pts',(1.67250335383248,1.,-1.00692206696387));
#31501=CARTESIAN_POINT('Ctrl Pts',(1.67648246776457,1.,-1.01123236493507));
#31502=CARTESIAN_POINT('Ctrl Pts',(1.6804428989482,1.,-1.01561026162787));
#31503=CARTESIAN_POINT('Ctrl Pts',(1.68440578021739,1.,-1.02006795074222));
#31504=CARTESIAN_POINT('Ctrl Pts',(1.68836910178475,1.,-1.02460180535272));
#31505=CARTESIAN_POINT('Ctrl Pts',(1.69231840863471,1.,-1.02919977579155));
#31506=CARTESIAN_POINT('Ctrl Pts',(1.69623414782769,1.,-1.03384646003587));
#31507=CARTESIAN_POINT('Ctrl Pts',(1.70010052930951,1.,-1.03852922490782));
#31508=CARTESIAN_POINT('Ctrl Pts',(1.70391338707969,1.,-1.04324363334546));
#31509=CARTESIAN_POINT('Ctrl Pts',(1.70767646263641,1.,-1.0479908540499));
#31510=CARTESIAN_POINT('Ctrl Pts',(1.71139783543986,1.,-1.05277517202854));
#31511=CARTESIAN_POINT('Ctrl Pts',(1.71508654427022,1.,-1.05760163192481));
#31512=CARTESIAN_POINT('Ctrl Pts',(1.71874858456908,1.,-1.0624732468065));
#31513=CARTESIAN_POINT('Ctrl Pts',(1.72238500928456,1.,-1.06738966975463));
#31514=CARTESIAN_POINT('Ctrl Pts',(1.72599406198489,1.,-1.07234866990252));
#31515=CARTESIAN_POINT('Ctrl Pts',(1.72957248977424,1.,-1.0773470373727));
#31516=CARTESIAN_POINT('Ctrl Pts',(1.73311705663407,1.,-1.08238162784749));
#31517=CARTESIAN_POINT('Ctrl Pts',(1.73662628326093,1.,-1.08745056285429));
#31518=CARTESIAN_POINT('Ctrl Pts',(1.74010053962252,1.,-1.09255329056496));
#31519=CARTESIAN_POINT('Ctrl Pts',(1.74354119236212,1.,-1.09768999241229));
#31520=CARTESIAN_POINT('Ctrl Pts',(1.74695004214924,1.,-1.10286118991144));
#31521=CARTESIAN_POINT('Ctrl Pts',(1.75032866075914,1.,-1.10806728183003));
#31522=CARTESIAN_POINT('Ctrl Pts',(1.75367772094617,1.,-1.11330807582542));
#31523=CARTESIAN_POINT('Ctrl Pts',(1.75699720772089,1.,-1.11858293216752));
#31524=CARTESIAN_POINT('Ctrl Pts',(1.76028671825084,1.,-1.12389096855078));
#31525=CARTESIAN_POINT('Ctrl Pts',(1.76354571966171,1.,-1.12923123555076));
#31526=CARTESIAN_POINT('Ctrl Pts',(1.76677384551883,1.,-1.13460291804635));
#31527=CARTESIAN_POINT('Ctrl Pts',(1.76997111386806,1.,-1.14000548337));
#31528=CARTESIAN_POINT('Ctrl Pts',(1.77313777896234,1.,-1.14543858226948));
#31529=CARTESIAN_POINT('Ctrl Pts',(1.77627422557034,1.,-1.15090197841531));
#31530=CARTESIAN_POINT('Ctrl Pts',(1.77938085564261,1.,-1.15639547194689));
#31531=CARTESIAN_POINT('Ctrl Pts',(1.78245795880949,1.,-1.16191881298458));
#31532=CARTESIAN_POINT('Ctrl Pts',(1.78550566040349,1.,-1.16747166312239));
#31533=CARTESIAN_POINT('Ctrl Pts',(1.78852398877523,1.,-1.17305363177265));
#31534=CARTESIAN_POINT('Ctrl Pts',(1.79151291552646,1.,-1.17866429440781));
#31535=CARTESIAN_POINT('Ctrl Pts',(1.79447240321572,1.,-1.18430321697471));
#31536=CARTESIAN_POINT('Ctrl Pts',(1.79740245923649,1.,-1.1899699793456));
#31537=CARTESIAN_POINT('Ctrl Pts',(1.80030314370121,1.,-1.19566418930405));
#31538=CARTESIAN_POINT('Ctrl Pts',(1.8031745483882,1.,-1.2013854893912));
#31539=CARTESIAN_POINT('Ctrl Pts',(1.80601678480772,1.,-1.20713356605519));
#31540=CARTESIAN_POINT('Ctrl Pts',(1.80882996916931,1.,-1.2129081570818));
#31541=CARTESIAN_POINT('Ctrl Pts',(1.81161420806172,1.,-1.2187090610323));
#31542=CARTESIAN_POINT('Ctrl Pts',(1.81436959209778,1.,-1.22453613304507));
#31543=CARTESIAN_POINT('Ctrl Pts',(1.81655087183054,1.,-1.22921864890975));
#31544=CARTESIAN_POINT('Ctrl Pts',(1.81817389920914,1.,-1.23274224526804));
#31545=CARTESIAN_POINT('Ctrl Pts',(1.81925017193531,1.,-1.23509651170384));
#31546=CARTESIAN_POINT('Ctrl Pts',(1.81978687191668,1.,-1.23627494547115));
#31547=CARTESIAN_POINT('',(1.5055822144029,0.,-0.892032620296855));
#31548=CARTESIAN_POINT('Origin',(0.,0.,0.));
#31549=CARTESIAN_POINT('',(1.60662857109684,1.,-0.693717979106306));
#31550=CARTESIAN_POINT('Origin',(0.,1.,0.));
#31551=CARTESIAN_POINT('',(1.60662857109684,0.,-0.693717979106308));
#31552=CARTESIAN_POINT('Ctrl Pts',(2.0698113262342,-1.,-0.745574324794401));
#31553=CARTESIAN_POINT('Ctrl Pts',(2.0698113262342,1.,-0.745574324794401));
#31554=CARTESIAN_POINT('Ctrl Pts',(2.06854248895728,-1.,-0.745832791378367));
#31555=CARTESIAN_POINT('Ctrl Pts',(2.06854248895728,1.,-0.745832791378367));
#31556=CARTESIAN_POINT('Ctrl Pts',(2.06600523016815,-1.,-0.746345871544201));
#31557=CARTESIAN_POINT('Ctrl Pts',(2.06600523016815,1.,-0.746345871544201));
#31558=CARTESIAN_POINT('Ctrl Pts',(2.06220058927826,-1.,-0.74710393278792));
#31559=CARTESIAN_POINT('Ctrl Pts',(2.06220058927826,1.,-0.74710393278792));
#31560=CARTESIAN_POINT('Ctrl Pts',(2.05713023031006,-1.,-0.748091554183803));
#31561=CARTESIAN_POINT('Ctrl Pts',(2.05713023031006,1.,-0.748091554183803));
#31562=CARTESIAN_POINT('Ctrl Pts',(2.05079645592154,-1.,-0.749287468665046));
#31563=CARTESIAN_POINT('Ctrl Pts',(2.05079645592154,1.,-0.749287468665046));
#31564=CARTESIAN_POINT('Ctrl Pts',(2.04446689147979,-1.,-0.750444657875576));
#31565=CARTESIAN_POINT('Ctrl Pts',(2.04446689147979,1.,-0.750444657875576));
#31566=CARTESIAN_POINT('Ctrl Pts',(2.03814160092099,-1.,-0.751562963361115));
#31567=CARTESIAN_POINT('Ctrl Pts',(2.03814160092099,1.,-0.751562963361115));
#31568=CARTESIAN_POINT('Ctrl Pts',(2.03182068456221,-1.,-0.752642180487211));
#31569=CARTESIAN_POINT('Ctrl Pts',(2.03182068456221,1.,-0.752642180487211));
#31570=CARTESIAN_POINT('Ctrl Pts',(2.02550428623313,-1.,-0.753682061112768));
#31571=CARTESIAN_POINT('Ctrl Pts',(2.02550428623313,1.,-0.753682061112768));
#31572=CARTESIAN_POINT('Ctrl Pts',(2.01919259405809,-1.,-0.754682330722816));
#31573=CARTESIAN_POINT('Ctrl Pts',(2.01919259405809,1.,-0.754682330722816));
#31574=CARTESIAN_POINT('Ctrl Pts',(2.01288584328084,-1.,-0.755642704957865));
#31575=CARTESIAN_POINT('Ctrl Pts',(2.01288584328084,1.,-0.755642704957865));
#31576=CARTESIAN_POINT('Ctrl Pts',(2.0065843158773,-1.,-0.756562904646671));
#31577=CARTESIAN_POINT('Ctrl Pts',(2.0065843158773,1.,-0.756562904646671));
#31578=CARTESIAN_POINT('Ctrl Pts',(2.00028834739178,-1.,-0.757442676862724));
#31579=CARTESIAN_POINT('Ctrl Pts',(2.00028834739178,1.,-0.757442676862724));
#31580=CARTESIAN_POINT('Ctrl Pts',(1.99399831098817,-1.,-0.758281796766761));
#31581=CARTESIAN_POINT('Ctrl Pts',(1.99399831098817,1.,-0.758281796766761));
#31582=CARTESIAN_POINT('Ctrl Pts',(1.98771456680874,-1.,-0.759080037802488));
#31583=CARTESIAN_POINT('Ctrl Pts',(1.98771456680874,1.,-0.759080037802488));
#31584=CARTESIAN_POINT('Ctrl Pts',(1.98143741418172,-1.,-0.75983714745219));
#31585=CARTESIAN_POINT('Ctrl Pts',(1.98143741418172,1.,-0.75983714745219));
#31586=CARTESIAN_POINT('Ctrl Pts',(1.97516705321494,-1.,-0.760552825409757));
#31587=CARTESIAN_POINT('Ctrl Pts',(1.97516705321494,1.,-0.760552825409757));
#31588=CARTESIAN_POINT('Ctrl Pts',(1.96890351582499,-1.,-0.761226690483821));
#31589=CARTESIAN_POINT('Ctrl Pts',(1.96890351582499,1.,-0.761226690483821));
#31590=CARTESIAN_POINT('Ctrl Pts',(1.96264672744186,-1.,-0.761858300014424));
#31591=CARTESIAN_POINT('Ctrl Pts',(1.96264672744186,1.,-0.761858300014424));
#31592=CARTESIAN_POINT('Ctrl Pts',(1.95639665309869,-1.,-0.762447203806179));
#31593=CARTESIAN_POINT('Ctrl Pts',(1.95639665309869,1.,-0.762447203806179));
#31594=CARTESIAN_POINT('Ctrl Pts',(1.95015342590024,-1.,-0.762992990878769));
#31595=CARTESIAN_POINT('Ctrl Pts',(1.95015342590024,1.,-0.762992990878769));
#31596=CARTESIAN_POINT('Ctrl Pts',(1.9439174661764,-1.,-0.763495333538629));
#31597=CARTESIAN_POINT('Ctrl Pts',(1.9439174661764,1.,-0.763495333538629));
#31598=CARTESIAN_POINT('Ctrl Pts',(1.93768964875886,-1.,-0.763954049121459));
#31599=CARTESIAN_POINT('Ctrl Pts',(1.93768964875886,1.,-0.763954049121459));
#31600=CARTESIAN_POINT('Ctrl Pts',(1.93147105496382,-1.,-0.764369010673941));
#31601=CARTESIAN_POINT('Ctrl Pts',(1.93147105496382,1.,-0.764369010673941));
#31602=CARTESIAN_POINT('Ctrl Pts',(1.92526263537048,-1.,-0.764740025488212));
#31603=CARTESIAN_POINT('Ctrl Pts',(1.92526263537048,1.,-0.764740025488212));
#31604=CARTESIAN_POINT('Ctrl Pts',(1.91906491634196,-1.,-0.765066729667089));
#31605=CARTESIAN_POINT('Ctrl Pts',(1.91906491634196,1.,-0.765066729667089));
#31606=CARTESIAN_POINT('Ctrl Pts',(1.91287765805169,-1.,-0.765348465884722));
#31607=CARTESIAN_POINT('Ctrl Pts',(1.91287765805169,1.,-0.765348465884722));
#31608=CARTESIAN_POINT('Ctrl Pts',(1.90669961402356,-1.,-0.765584196937919));
#31609=CARTESIAN_POINT('Ctrl Pts',(1.90669961402356,1.,-0.765584196937919));
#31610=CARTESIAN_POINT('Ctrl Pts',(1.90052930393596,-1.,-0.765772772593386));
#31611=CARTESIAN_POINT('Ctrl Pts',(1.90052930393596,1.,-0.765772772593386));
#31612=CARTESIAN_POINT('Ctrl Pts',(1.89436577771388,-1.,-0.765913193856978));
#31613=CARTESIAN_POINT('Ctrl Pts',(1.89436577771388,1.,-0.765913193856978));
#31614=CARTESIAN_POINT('Ctrl Pts',(1.88820926433409,-1.,-0.766004837062091));
#31615=CARTESIAN_POINT('Ctrl Pts',(1.88820926433409,1.,-0.766004837062091));
#31616=CARTESIAN_POINT('Ctrl Pts',(1.88206215302561,-1.,-0.766047794851865));
#31617=CARTESIAN_POINT('Ctrl Pts',(1.88206215302561,1.,-0.766047794851865));
#31618=CARTESIAN_POINT('Ctrl Pts',(1.87592888967883,-1.,-0.766042837036744));
#31619=CARTESIAN_POINT('Ctrl Pts',(1.87592888967883,1.,-0.766042837036744));
#31620=CARTESIAN_POINT('Ctrl Pts',(1.86981398314341,-1.,-0.765990708546091));
#31621=CARTESIAN_POINT('Ctrl Pts',(1.86981398314341,1.,-0.765990708546091));
#31622=CARTESIAN_POINT('Ctrl Pts',(1.86372027063312,-1.,-0.765891519092547));
#31623=CARTESIAN_POINT('Ctrl Pts',(1.86372027063312,1.,-0.765891519092547));
#31624=CARTESIAN_POINT('Ctrl Pts',(1.85764741390394,-1.,-0.765744212909319));
#31625=CARTESIAN_POINT('Ctrl Pts',(1.85764741390394,1.,-0.765744212909319));
#31626=CARTESIAN_POINT('Ctrl Pts',(1.85158945130063,-1.,-0.765545710619063));
#31627=CARTESIAN_POINT('Ctrl Pts',(1.85158945130063,1.,-0.765545710619063));
#31628=CARTESIAN_POINT('Ctrl Pts',(1.84553698875924,-1.,-0.765291664862029));
#31629=CARTESIAN_POINT('Ctrl Pts',(1.84553698875924,1.,-0.765291664862029));
#31630=CARTESIAN_POINT('Ctrl Pts',(1.83948181064835,-1.,-0.764978057881738));
#31631=CARTESIAN_POINT('Ctrl Pts',(1.83948181064835,1.,-0.764978057881738));
#31632=CARTESIAN_POINT('Ctrl Pts',(1.83342077227142,-1.,-0.764602549687853));
#31633=CARTESIAN_POINT('Ctrl Pts',(1.83342077227142,1.,-0.764602549687853));
#31634=CARTESIAN_POINT('Ctrl Pts',(1.82735991200065,-1.,-0.764165902605995));
#31635=CARTESIAN_POINT('Ctrl Pts',(1.82735991200065,1.,-0.764165902605995));
#31636=CARTESIAN_POINT('Ctrl Pts',(1.82131873145266,-1.,-0.763673465462727));
#31637=CARTESIAN_POINT('Ctrl Pts',(1.82131873145266,1.,-0.763673465462727));
#31638=CARTESIAN_POINT('Ctrl Pts',(1.8153211840553,-1.,-0.763132003836634));
#31639=CARTESIAN_POINT('Ctrl Pts',(1.8153211840553,1.,-0.763132003836634));
#31640=CARTESIAN_POINT('Ctrl Pts',(1.80938551463965,-1.,-0.762546129463938));
#31641=CARTESIAN_POINT('Ctrl Pts',(1.80938551463965,1.,-0.762546129463938));
#31642=CARTESIAN_POINT('Ctrl Pts',(1.80351583877342,-1.,-0.761915336443547));
#31643=CARTESIAN_POINT('Ctrl Pts',(1.80351583877342,1.,-0.761915336443547));
#31644=CARTESIAN_POINT('Ctrl Pts',(1.79768986997783,-1.,-0.761229695230558));
#31645=CARTESIAN_POINT('Ctrl Pts',(1.79768986997783,1.,-0.761229695230558));
#31646=CARTESIAN_POINT('Ctrl Pts',(1.7918581561088,-1.,-0.760469555880749));
#31647=CARTESIAN_POINT('Ctrl Pts',(1.7918581561088,1.,-0.760469555880749));
#31648=CARTESIAN_POINT('Ctrl Pts',(1.78596964884604,-1.,-0.75961440111019));
#31649=CARTESIAN_POINT('Ctrl Pts',(1.78596964884604,1.,-0.75961440111019));
#31650=CARTESIAN_POINT('Ctrl Pts',(1.77999411220945,-1.,-0.758650626677519));
#31651=CARTESIAN_POINT('Ctrl Pts',(1.77999411220945,1.,-0.758650626677519));
#31652=CARTESIAN_POINT('Ctrl Pts',(1.77394167108292,-1.,-0.757578264077029));
#31653=CARTESIAN_POINT('Ctrl Pts',(1.77394167108292,1.,-0.757578264077029));
#31654=CARTESIAN_POINT('Ctrl Pts',(1.76789396002998,-1.,-0.75642189602781));
#31655=CARTESIAN_POINT('Ctrl Pts',(1.76789396002998,1.,-0.75642189602781));
#31656=CARTESIAN_POINT('Ctrl Pts',(1.76197817240128,-1.,-0.755220979974462));
#31657=CARTESIAN_POINT('Ctrl Pts',(1.76197817240128,1.,-0.755220979974462));
#31658=CARTESIAN_POINT('Ctrl Pts',(1.75631083600019,-1.,-0.754009254027829));
#31659=CARTESIAN_POINT('Ctrl Pts',(1.75631083600019,1.,-0.754009254027829));
#31660=CARTESIAN_POINT('Ctrl Pts',(1.75095139468794,-1.,-0.752797683531314));
#31661=CARTESIAN_POINT('Ctrl Pts',(1.75095139468794,1.,-0.752797683531314));
#31662=CARTESIAN_POINT('Ctrl Pts',(1.74585086852502,-1.,-0.751555614164483));
#31663=CARTESIAN_POINT('Ctrl Pts',(1.74585086852502,1.,-0.751555614164483));
#31664=CARTESIAN_POINT('Ctrl Pts',(1.74080458267114,-1.,-0.75019343598125));
#31665=CARTESIAN_POINT('Ctrl Pts',(1.74080458267114,1.,-0.75019343598125));
#31666=CARTESIAN_POINT('Ctrl Pts',(1.7355035168033,-1.,-0.74858246295687));
#31667=CARTESIAN_POINT('Ctrl Pts',(1.7355035168033,1.,-0.74858246295687));
#31668=CARTESIAN_POINT('Ctrl Pts',(1.72958533647714,-1.,-0.746574710097752));
#31669=CARTESIAN_POINT('Ctrl Pts',(1.72958533647714,1.,-0.746574710097752));
#31670=CARTESIAN_POINT('Ctrl Pts',(1.72268229916769,-1.,-0.744021445433094));
#31671=CARTESIAN_POINT('Ctrl Pts',(1.72268229916769,1.,-0.744021445433094));
#31672=CARTESIAN_POINT('Ctrl Pts',(1.71447789751001,-1.,-0.74079516202821));
#31673=CARTESIAN_POINT('Ctrl Pts',(1.71447789751001,1.,-0.74079516202821));
#31674=CARTESIAN_POINT('Ctrl Pts',(1.70473309004249,-1.,-0.736799665716932));
#31675=CARTESIAN_POINT('Ctrl Pts',(1.70473309004249,1.,-0.736799665716932));
#31676=CARTESIAN_POINT('Ctrl Pts',(1.69326921972915,-1.,-0.731963238685357));
#31677=CARTESIAN_POINT('Ctrl Pts',(1.69326921972915,1.,-0.731963238685357));
#31678=CARTESIAN_POINT('Ctrl Pts',(1.67996158451922,-1.,-0.726235967982445));
#31679=CARTESIAN_POINT('Ctrl Pts',(1.67996158451922,1.,-0.726235967982445));
#31680=CARTESIAN_POINT('Ctrl Pts',(1.66472880551777,-1.,-0.71958543378795));
#31681=CARTESIAN_POINT('Ctrl Pts',(1.66472880551777,1.,-0.71958543378795));
#31682=CARTESIAN_POINT('Ctrl Pts',(1.64752408828442,-1.,-0.711993139340448));
#31683=CARTESIAN_POINT('Ctrl Pts',(1.64752408828442,1.,-0.711993139340448));
#31684=CARTESIAN_POINT('Ctrl Pts',(1.6321654166204,-1.,-0.705159151977294));
#31685=CARTESIAN_POINT('Ctrl Pts',(1.6321654166204,1.,-0.705159151977294));
#31686=CARTESIAN_POINT('Ctrl Pts',(1.61974673471117,-1.,-0.699605146398837));
#31687=CARTESIAN_POINT('Ctrl Pts',(1.61974673471117,1.,-0.699605146398837));
#31688=CARTESIAN_POINT('Ctrl Pts',(1.61106790957619,-1.,-0.69571209787897));
#31689=CARTESIAN_POINT('Ctrl Pts',(1.61106790957619,1.,-0.69571209787897));
#31690=CARTESIAN_POINT('Ctrl Pts',(1.60662857109684,-1.,-0.693717979106306));
#31691=CARTESIAN_POINT('Ctrl Pts',(1.60662857109684,1.,-0.693717979106306));
#31692=CARTESIAN_POINT('',(2.0698113262342,1.,-0.745574324794401));
#31693=CARTESIAN_POINT('Ctrl Pts',(2.0698113262342,1.,-0.745574324794401));
#31694=CARTESIAN_POINT('Ctrl Pts',(2.06854248895728,1.,-0.745832791378367));
#31695=CARTESIAN_POINT('Ctrl Pts',(2.06600523016815,1.,-0.746345871544201));
#31696=CARTESIAN_POINT('Ctrl Pts',(2.06220058927826,1.,-0.74710393278792));
#31697=CARTESIAN_POINT('Ctrl Pts',(2.05713023031006,1.,-0.748091554183803));
#31698=CARTESIAN_POINT('Ctrl Pts',(2.05079645592154,1.,-0.749287468665046));
#31699=CARTESIAN_POINT('Ctrl Pts',(2.04446689147979,1.,-0.750444657875576));
#31700=CARTESIAN_POINT('Ctrl Pts',(2.03814160092099,1.,-0.751562963361115));
#31701=CARTESIAN_POINT('Ctrl Pts',(2.03182068456221,1.,-0.752642180487211));
#31702=CARTESIAN_POINT('Ctrl Pts',(2.02550428623313,1.,-0.753682061112768));
#31703=CARTESIAN_POINT('Ctrl Pts',(2.01919259405809,1.,-0.754682330722816));
#31704=CARTESIAN_POINT('Ctrl Pts',(2.01288584328084,1.,-0.755642704957865));
#31705=CARTESIAN_POINT('Ctrl Pts',(2.0065843158773,1.,-0.756562904646671));
#31706=CARTESIAN_POINT('Ctrl Pts',(2.00028834739178,1.,-0.757442676862724));
#31707=CARTESIAN_POINT('Ctrl Pts',(1.99399831098817,1.,-0.758281796766761));
#31708=CARTESIAN_POINT('Ctrl Pts',(1.98771456680874,1.,-0.759080037802488));
#31709=CARTESIAN_POINT('Ctrl Pts',(1.98143741418172,1.,-0.75983714745219));
#31710=CARTESIAN_POINT('Ctrl Pts',(1.97516705321494,1.,-0.760552825409757));
#31711=CARTESIAN_POINT('Ctrl Pts',(1.96890351582499,1.,-0.761226690483821));
#31712=CARTESIAN_POINT('Ctrl Pts',(1.96264672744186,1.,-0.761858300014424));
#31713=CARTESIAN_POINT('Ctrl Pts',(1.95639665309869,1.,-0.762447203806179));
#31714=CARTESIAN_POINT('Ctrl Pts',(1.95015342590024,1.,-0.762992990878769));
#31715=CARTESIAN_POINT('Ctrl Pts',(1.9439174661764,1.,-0.763495333538629));
#31716=CARTESIAN_POINT('Ctrl Pts',(1.93768964875886,1.,-0.763954049121459));
#31717=CARTESIAN_POINT('Ctrl Pts',(1.93147105496382,1.,-0.764369010673941));
#31718=CARTESIAN_POINT('Ctrl Pts',(1.92526263537048,1.,-0.764740025488212));
#31719=CARTESIAN_POINT('Ctrl Pts',(1.91906491634196,1.,-0.765066729667089));
#31720=CARTESIAN_POINT('Ctrl Pts',(1.91287765805169,1.,-0.765348465884722));
#31721=CARTESIAN_POINT('Ctrl Pts',(1.90669961402356,1.,-0.765584196937919));
#31722=CARTESIAN_POINT('Ctrl Pts',(1.90052930393596,1.,-0.765772772593386));
#31723=CARTESIAN_POINT('Ctrl Pts',(1.89436577771388,1.,-0.765913193856978));
#31724=CARTESIAN_POINT('Ctrl Pts',(1.88820926433409,1.,-0.766004837062091));
#31725=CARTESIAN_POINT('Ctrl Pts',(1.88206215302561,1.,-0.766047794851865));
#31726=CARTESIAN_POINT('Ctrl Pts',(1.87592888967883,1.,-0.766042837036744));
#31727=CARTESIAN_POINT('Ctrl Pts',(1.86981398314341,1.,-0.765990708546091));
#31728=CARTESIAN_POINT('Ctrl Pts',(1.86372027063312,1.,-0.765891519092547));
#31729=CARTESIAN_POINT('Ctrl Pts',(1.85764741390394,1.,-0.765744212909319));
#31730=CARTESIAN_POINT('Ctrl Pts',(1.85158945130063,1.,-0.765545710619063));
#31731=CARTESIAN_POINT('Ctrl Pts',(1.84553698875924,1.,-0.765291664862029));
#31732=CARTESIAN_POINT('Ctrl Pts',(1.83948181064835,1.,-0.764978057881738));
#31733=CARTESIAN_POINT('Ctrl Pts',(1.83342077227142,1.,-0.764602549687853));
#31734=CARTESIAN_POINT('Ctrl Pts',(1.82735991200065,1.,-0.764165902605995));
#31735=CARTESIAN_POINT('Ctrl Pts',(1.82131873145266,1.,-0.763673465462727));
#31736=CARTESIAN_POINT('Ctrl Pts',(1.8153211840553,1.,-0.763132003836634));
#31737=CARTESIAN_POINT('Ctrl Pts',(1.80938551463965,1.,-0.762546129463938));
#31738=CARTESIAN_POINT('Ctrl Pts',(1.80351583877342,1.,-0.761915336443547));
#31739=CARTESIAN_POINT('Ctrl Pts',(1.79768986997783,1.,-0.761229695230558));
#31740=CARTESIAN_POINT('Ctrl Pts',(1.7918581561088,1.,-0.760469555880749));
#31741=CARTESIAN_POINT('Ctrl Pts',(1.78596964884604,1.,-0.75961440111019));
#31742=CARTESIAN_POINT('Ctrl Pts',(1.77999411220945,1.,-0.758650626677519));
#31743=CARTESIAN_POINT('Ctrl Pts',(1.77394167108292,1.,-0.757578264077029));
#31744=CARTESIAN_POINT('Ctrl Pts',(1.76789396002998,1.,-0.75642189602781));
#31745=CARTESIAN_POINT('Ctrl Pts',(1.76197817240128,1.,-0.755220979974462));
#31746=CARTESIAN_POINT('Ctrl Pts',(1.75631083600019,1.,-0.754009254027829));
#31747=CARTESIAN_POINT('Ctrl Pts',(1.75095139468794,1.,-0.752797683531314));
#31748=CARTESIAN_POINT('Ctrl Pts',(1.74585086852502,1.,-0.751555614164483));
#31749=CARTESIAN_POINT('Ctrl Pts',(1.74080458267114,1.,-0.75019343598125));
#31750=CARTESIAN_POINT('Ctrl Pts',(1.7355035168033,1.,-0.74858246295687));
#31751=CARTESIAN_POINT('Ctrl Pts',(1.72958533647714,1.,-0.746574710097752));
#31752=CARTESIAN_POINT('Ctrl Pts',(1.72268229916769,1.,-0.744021445433094));
#31753=CARTESIAN_POINT('Ctrl Pts',(1.71447789751001,1.,-0.74079516202821));
#31754=CARTESIAN_POINT('Ctrl Pts',(1.70473309004249,1.,-0.736799665716932));
#31755=CARTESIAN_POINT('Ctrl Pts',(1.69326921972915,1.,-0.731963238685357));
#31756=CARTESIAN_POINT('Ctrl Pts',(1.67996158451922,1.,-0.726235967982445));
#31757=CARTESIAN_POINT('Ctrl Pts',(1.66472880551777,1.,-0.71958543378795));
#31758=CARTESIAN_POINT('Ctrl Pts',(1.64752408828442,1.,-0.711993139340448));
#31759=CARTESIAN_POINT('Ctrl Pts',(1.6321654166204,1.,-0.705159151977294));
#31760=CARTESIAN_POINT('Ctrl Pts',(1.61974673471117,1.,-0.699605146398837));
#31761=CARTESIAN_POINT('Ctrl Pts',(1.61106790957619,1.,-0.69571209787897));
#31762=CARTESIAN_POINT('Ctrl Pts',(1.60662857109684,1.,-0.693717979106306));
#31763=CARTESIAN_POINT('',(2.0698113262342,0.,-0.745574324794401));
#31764=CARTESIAN_POINT('Origin',(2.11275013067528,0.,-0.61342227326009));
#31765=CARTESIAN_POINT('',(2.11275013067528,1.,-0.61342227326009));
#31766=CARTESIAN_POINT('',(2.0698113262342,1.,-0.745574324794401));
#31767=CARTESIAN_POINT('',(2.11275013067528,0.,-0.61342227326009));
#31768=CARTESIAN_POINT('Ctrl Pts',(1.7075470150345,-1.,-0.383122945602004));
#31769=CARTESIAN_POINT('Ctrl Pts',(1.7075470150345,1.,-0.383122945602004));
#31770=CARTESIAN_POINT('Ctrl Pts',(1.71231062891958,-1.,-0.384119047315542));
#31771=CARTESIAN_POINT('Ctrl Pts',(1.71231062891958,1.,-0.384119047315542));
#31772=CARTESIAN_POINT('Ctrl Pts',(1.72162022246158,-1.,-0.38607079032701));
#31773=CARTESIAN_POINT('Ctrl Pts',(1.72162022246158,1.,-0.38607079032701));
#31774=CARTESIAN_POINT('Ctrl Pts',(1.7349317097561,-1.,-0.388877023509192));
#31775=CARTESIAN_POINT('Ctrl Pts',(1.7349317097561,1.,-0.388877023509192));
#31776=CARTESIAN_POINT('Ctrl Pts',(1.75137405313962,-1.,-0.392375812294307));
#31777=CARTESIAN_POINT('Ctrl Pts',(1.75137405313962,1.,-0.392375812294307));
#31778=CARTESIAN_POINT('Ctrl Pts',(1.7697556004756,-1.,-0.39634619612042));
#31779=CARTESIAN_POINT('Ctrl Pts',(1.7697556004756,1.,-0.39634619612042));
#31780=CARTESIAN_POINT('Ctrl Pts',(1.78598826347533,-1.,-0.399919403783081));
#31781=CARTESIAN_POINT('Ctrl Pts',(1.78598826347533,1.,-0.399919403783081));
#31782=CARTESIAN_POINT('Ctrl Pts',(1.80012077176221,-1.,-0.403107976170441));
#31783=CARTESIAN_POINT('Ctrl Pts',(1.80012077176221,1.,-0.403107976170441));
#31784=CARTESIAN_POINT('Ctrl Pts',(1.81223801813988,-1.,-0.405933518411838));
#31785=CARTESIAN_POINT('Ctrl Pts',(1.81223801813988,1.,-0.405933518411838));
#31786=CARTESIAN_POINT('Ctrl Pts',(1.8224702267854,-1.,-0.408428948108534));
#31787=CARTESIAN_POINT('Ctrl Pts',(1.8224702267854,1.,-0.408428948108534));
#31788=CARTESIAN_POINT('Ctrl Pts',(1.83100408895216,-1.,-0.410641256301675));
#31789=CARTESIAN_POINT('Ctrl Pts',(1.83100408895216,1.,-0.410641256301675));
#31790=CARTESIAN_POINT('Ctrl Pts',(1.83808953475839,-1.,-0.412633125322162));
#31791=CARTESIAN_POINT('Ctrl Pts',(1.83808953475839,1.,-0.412633125322162));
#31792=CARTESIAN_POINT('Ctrl Pts',(1.8440575707371,-1.,-0.41448743825434));
#31793=CARTESIAN_POINT('Ctrl Pts',(1.8440575707371,1.,-0.41448743825434));
#31794=CARTESIAN_POINT('Ctrl Pts',(1.84929312929882,-1.,-0.416300022038864));
#31795=CARTESIAN_POINT('Ctrl Pts',(1.84929312929882,1.,-0.416300022038864));
#31796=CARTESIAN_POINT('Ctrl Pts',(1.85417632856234,-1.,-0.418164129143534));
#31797=CARTESIAN_POINT('Ctrl Pts',(1.85417632856234,1.,-0.418164129143534));
#31798=CARTESIAN_POINT('Ctrl Pts',(1.85903281096686,-1.,-0.42015728797562));
#31799=CARTESIAN_POINT('Ctrl Pts',(1.85903281096686,1.,-0.42015728797562));
#31800=CARTESIAN_POINT('Ctrl Pts',(1.86408083334028,-1.,-0.422327307418275));
#31801=CARTESIAN_POINT('Ctrl Pts',(1.86408083334028,1.,-0.422327307418275));
#31802=CARTESIAN_POINT('Ctrl Pts',(1.86937803944323,-1.,-0.424678177291359));
#31803=CARTESIAN_POINT('Ctrl Pts',(1.86937803944323,1.,-0.424678177291359));
#31804=CARTESIAN_POINT('Ctrl Pts',(1.87486989291484,-1.,-0.427183828519102));
#31805=CARTESIAN_POINT('Ctrl Pts',(1.87486989291484,1.,-0.427183828519102));
#31806=CARTESIAN_POINT('Ctrl Pts',(1.88044229001832,-1.,-0.429803062482345));
#31807=CARTESIAN_POINT('Ctrl Pts',(1.88044229001832,1.,-0.429803062482345));
#31808=CARTESIAN_POINT('Ctrl Pts',(1.88596913666793,-1.,-0.432493038548748));
#31809=CARTESIAN_POINT('Ctrl Pts',(1.88596913666793,1.,-0.432493038548748));
#31810=CARTESIAN_POINT('Ctrl Pts',(1.89136993975504,-1.,-0.435225660963383));
#31811=CARTESIAN_POINT('Ctrl Pts',(1.89136993975504,1.,-0.435225660963383));
#31812=CARTESIAN_POINT('Ctrl Pts',(1.89663648956466,-1.,-0.437995003948244));
#31813=CARTESIAN_POINT('Ctrl Pts',(1.89663648956466,1.,-0.437995003948244));
#31814=CARTESIAN_POINT('Ctrl Pts',(1.90180124389086,-1.,-0.440807833704038));
#31815=CARTESIAN_POINT('Ctrl Pts',(1.90180124389086,1.,-0.440807833704038));
#31816=CARTESIAN_POINT('Ctrl Pts',(1.90691756144898,-1.,-0.443677556849151));
#31817=CARTESIAN_POINT('Ctrl Pts',(1.90691756144898,1.,-0.443677556849151));
#31818=CARTESIAN_POINT('Ctrl Pts',(1.9120369998112,-1.,-0.446617343485711));
#31819=CARTESIAN_POINT('Ctrl Pts',(1.9120369998112,1.,-0.446617343485711));
#31820=CARTESIAN_POINT('Ctrl Pts',(1.91718342555755,-1.,-0.449632260106662));
#31821=CARTESIAN_POINT('Ctrl Pts',(1.91718342555755,1.,-0.449632260106662));
#31822=CARTESIAN_POINT('Ctrl Pts',(1.92235380648502,-1.,-0.452719478359433));
#31823=CARTESIAN_POINT('Ctrl Pts',(1.92235380648502,1.,-0.452719478359433));
#31824=CARTESIAN_POINT('Ctrl Pts',(1.92753067150476,-1.,-0.455872005174371));
#31825=CARTESIAN_POINT('Ctrl Pts',(1.92753067150476,1.,-0.455872005174371));
#31826=CARTESIAN_POINT('Ctrl Pts',(1.93269066517934,-1.,-0.459081234547926));
#31827=CARTESIAN_POINT('Ctrl Pts',(1.93269066517934,1.,-0.459081234547926));
#31828=CARTESIAN_POINT('Ctrl Pts',(1.93781486640821,-1.,-0.462340031009057));
#31829=CARTESIAN_POINT('Ctrl Pts',(1.93781486640821,1.,-0.462340031009057));
#31830=CARTESIAN_POINT('Ctrl Pts',(1.9428979419619,-1.,-0.46564546202603));
#31831=CARTESIAN_POINT('Ctrl Pts',(1.9428979419619,1.,-0.46564546202603));
#31832=CARTESIAN_POINT('Ctrl Pts',(1.94794381136514,-1.,-0.468997482913135));
#31833=CARTESIAN_POINT('Ctrl Pts',(1.94794381136514,1.,-0.468997482913135));
#31834=CARTESIAN_POINT('Ctrl Pts',(1.95296148278133,-1.,-0.472397672264072));
#31835=CARTESIAN_POINT('Ctrl Pts',(1.95296148278133,1.,-0.472397672264072));
#31836=CARTESIAN_POINT('Ctrl Pts',(1.95796111148177,-1.,-0.475848034683176));
#31837=CARTESIAN_POINT('Ctrl Pts',(1.95796111148177,1.,-0.475848034683176));
#31838=CARTESIAN_POINT('Ctrl Pts',(1.96294933055943,-1.,-0.479349583074855));
#31839=CARTESIAN_POINT('Ctrl Pts',(1.96294933055943,1.,-0.479349583074855));
#31840=CARTESIAN_POINT('Ctrl Pts',(1.96792703422362,-1.,-0.482901662120691));
#31841=CARTESIAN_POINT('Ctrl Pts',(1.96792703422362,1.,-0.482901662120691));
#31842=CARTESIAN_POINT('Ctrl Pts',(1.97289186263272,-1.,-0.486502692907659));
#31843=CARTESIAN_POINT('Ctrl Pts',(1.97289186263272,1.,-0.486502692907659));
#31844=CARTESIAN_POINT('Ctrl Pts',(1.97783973019229,-1.,-0.490150627860953));
#31845=CARTESIAN_POINT('Ctrl Pts',(1.97783973019229,1.,-0.490150627860953));
#31846=CARTESIAN_POINT('Ctrl Pts',(1.98276658761821,-1.,-0.493843476541495));
#31847=CARTESIAN_POINT('Ctrl Pts',(1.98276658761821,1.,-0.493843476541495));
#31848=CARTESIAN_POINT('Ctrl Pts',(1.98767044752932,-1.,-0.497579909545574));
#31849=CARTESIAN_POINT('Ctrl Pts',(1.98767044752932,1.,-0.497579909545574));
#31850=CARTESIAN_POINT('Ctrl Pts',(1.99255149126155,-1.,-0.501359287727146));
#31851=CARTESIAN_POINT('Ctrl Pts',(1.99255149126155,1.,-0.501359287727146));
#31852=CARTESIAN_POINT('Ctrl Pts',(1.99741107463572,-1.,-0.505181361323026));
#31853=CARTESIAN_POINT('Ctrl Pts',(1.99741107463572,1.,-0.505181361323026));
#31854=CARTESIAN_POINT('Ctrl Pts',(2.00225107134734,-1.,-0.509046069886157));
#31855=CARTESIAN_POINT('Ctrl Pts',(2.00225107134734,1.,-0.509046069886157));
#31856=CARTESIAN_POINT('Ctrl Pts',(2.00707309946949,-1.,-0.512953306961793));
#31857=CARTESIAN_POINT('Ctrl Pts',(2.00707309946949,1.,-0.512953306961793));
#31858=CARTESIAN_POINT('Ctrl Pts',(2.01187773939242,-1.,-0.516902681728687));
#31859=CARTESIAN_POINT('Ctrl Pts',(2.01187773939242,1.,-0.516902681728687));
#31860=CARTESIAN_POINT('Ctrl Pts',(2.01666477917286,-1.,-0.520893590399371));
#31861=CARTESIAN_POINT('Ctrl Pts',(2.01666477917286,1.,-0.520893590399371));
#31862=CARTESIAN_POINT('Ctrl Pts',(2.02143356304698,-1.,-0.524925318333476));
#31863=CARTESIAN_POINT('Ctrl Pts',(2.02143356304698,1.,-0.524925318333476));
#31864=CARTESIAN_POINT('Ctrl Pts',(2.0261832908329,-1.,-0.528997127241914));
#31865=CARTESIAN_POINT('Ctrl Pts',(2.0261832908329,1.,-0.528997127241914));
#31866=CARTESIAN_POINT('Ctrl Pts',(2.03091336214426,-1.,-0.533108355132977));
#31867=CARTESIAN_POINT('Ctrl Pts',(2.03091336214426,1.,-0.533108355132977));
#31868=CARTESIAN_POINT('Ctrl Pts',(2.03562362954037,-1.,-0.537258489833262));
#31869=CARTESIAN_POINT('Ctrl Pts',(2.03562362954037,1.,-0.537258489833262));
#31870=CARTESIAN_POINT('Ctrl Pts',(2.04031422690527,-1.,-0.541447120615659));
#31871=CARTESIAN_POINT('Ctrl Pts',(2.04031422690527,1.,-0.541447120615659));
#31872=CARTESIAN_POINT('Ctrl Pts',(2.04498544714588,-1.,-0.54567390381743));
#31873=CARTESIAN_POINT('Ctrl Pts',(2.04498544714588,1.,-0.54567390381743));
#31874=CARTESIAN_POINT('Ctrl Pts',(2.04963761077958,-1.,-0.549938525150295));
#31875=CARTESIAN_POINT('Ctrl Pts',(2.04963761077958,1.,-0.549938525150295));
#31876=CARTESIAN_POINT('Ctrl Pts',(2.05427091604413,-1.,-0.554240657463906));
#31877=CARTESIAN_POINT('Ctrl Pts',(2.05427091604413,1.,-0.554240657463906));
#31878=CARTESIAN_POINT('Ctrl Pts',(2.05888537756462,-1.,-0.558579940185152));
#31879=CARTESIAN_POINT('Ctrl Pts',(2.05888537756462,1.,-0.558579940185152));
#31880=CARTESIAN_POINT('Ctrl Pts',(2.06348090160589,-1.,-0.562955993082262));
#31881=CARTESIAN_POINT('Ctrl Pts',(2.06348090160589,1.,-0.562955993082262));
#31882=CARTESIAN_POINT('Ctrl Pts',(2.06805732997334,-1.,-0.567368421181087));
#31883=CARTESIAN_POINT('Ctrl Pts',(2.06805732997334,1.,-0.567368421181087));
#31884=CARTESIAN_POINT('Ctrl Pts',(2.07261449292824,-1.,-0.571816823242603));
#31885=CARTESIAN_POINT('Ctrl Pts',(2.07261449292824,1.,-0.571816823242603));
#31886=CARTESIAN_POINT('Ctrl Pts',(2.07715226767559,-1.,-0.576300797416845));
#31887=CARTESIAN_POINT('Ctrl Pts',(2.07715226767559,1.,-0.576300797416845));
#31888=CARTESIAN_POINT('Ctrl Pts',(2.08167059018418,-1.,-0.580819952108064));
#31889=CARTESIAN_POINT('Ctrl Pts',(2.08167059018418,1.,-0.580819952108064));
#31890=CARTESIAN_POINT('Ctrl Pts',(2.08616943727951,-1.,-0.585373918991617));
#31891=CARTESIAN_POINT('Ctrl Pts',(2.08616943727951,1.,-0.585373918991617));
#31892=CARTESIAN_POINT('Ctrl Pts',(2.09064881812129,-1.,-0.589962365403406));
#31893=CARTESIAN_POINT('Ctrl Pts',(2.09064881812129,1.,-0.589962365403406));
#31894=CARTESIAN_POINT('Ctrl Pts',(2.0951087622027,-1.,-0.594585006052162));
#31895=CARTESIAN_POINT('Ctrl Pts',(2.0951087622027,1.,-0.594585006052162));
#31896=CARTESIAN_POINT('Ctrl Pts',(2.0995493086477,-1.,-0.599241616420534));
#31897=CARTESIAN_POINT('Ctrl Pts',(2.0995493086477,1.,-0.599241616420534));
#31898=CARTESIAN_POINT('Ctrl Pts',(2.10397049886949,-1.,-0.60393203073603));
#31899=CARTESIAN_POINT('Ctrl Pts',(2.10397049886949,1.,-0.60393203073603));
#31900=CARTESIAN_POINT('Ctrl Pts',(2.1074919961518,-1.,-0.607711315454876));
#31901=CARTESIAN_POINT('Ctrl Pts',(2.1074919961518,1.,-0.607711315454876));
#31902=CARTESIAN_POINT('Ctrl Pts',(2.11012443807238,-1.,-0.610560911689899));
#31903=CARTESIAN_POINT('Ctrl Pts',(2.11012443807238,1.,-0.610560911689899));
#31904=CARTESIAN_POINT('Ctrl Pts',(2.11187554259986,-1.,-0.6124673655618));
#31905=CARTESIAN_POINT('Ctrl Pts',(2.11187554259986,1.,-0.6124673655618));
#31906=CARTESIAN_POINT('Ctrl Pts',(2.11275013067528,-1.,-0.61342227326009));
#31907=CARTESIAN_POINT('Ctrl Pts',(2.11275013067528,1.,-0.61342227326009));
#31908=CARTESIAN_POINT('',(1.7075470150345,1.,-0.383122945602004));
#31909=CARTESIAN_POINT('Ctrl Pts',(1.7075470150345,1.,-0.383122945602004));
#31910=CARTESIAN_POINT('Ctrl Pts',(1.71231062891958,1.,-0.384119047315542));
#31911=CARTESIAN_POINT('Ctrl Pts',(1.72162022246158,1.,-0.38607079032701));
#31912=CARTESIAN_POINT('Ctrl Pts',(1.7349317097561,1.,-0.388877023509192));
#31913=CARTESIAN_POINT('Ctrl Pts',(1.75137405313962,1.,-0.392375812294307));
#31914=CARTESIAN_POINT('Ctrl Pts',(1.7697556004756,1.,-0.39634619612042));
#31915=CARTESIAN_POINT('Ctrl Pts',(1.78598826347533,1.,-0.399919403783081));
#31916=CARTESIAN_POINT('Ctrl Pts',(1.80012077176221,1.,-0.403107976170441));
#31917=CARTESIAN_POINT('Ctrl Pts',(1.81223801813988,1.,-0.405933518411838));
#31918=CARTESIAN_POINT('Ctrl Pts',(1.8224702267854,1.,-0.408428948108534));
#31919=CARTESIAN_POINT('Ctrl Pts',(1.83100408895216,1.,-0.410641256301675));
#31920=CARTESIAN_POINT('Ctrl Pts',(1.83808953475839,1.,-0.412633125322162));
#31921=CARTESIAN_POINT('Ctrl Pts',(1.8440575707371,1.,-0.41448743825434));
#31922=CARTESIAN_POINT('Ctrl Pts',(1.84929312929882,1.,-0.416300022038864));
#31923=CARTESIAN_POINT('Ctrl Pts',(1.85417632856234,1.,-0.418164129143534));
#31924=CARTESIAN_POINT('Ctrl Pts',(1.85903281096686,1.,-0.42015728797562));
#31925=CARTESIAN_POINT('Ctrl Pts',(1.86408083334028,1.,-0.422327307418275));
#31926=CARTESIAN_POINT('Ctrl Pts',(1.86937803944323,1.,-0.424678177291359));
#31927=CARTESIAN_POINT('Ctrl Pts',(1.87486989291484,1.,-0.427183828519102));
#31928=CARTESIAN_POINT('Ctrl Pts',(1.88044229001832,1.,-0.429803062482345));
#31929=CARTESIAN_POINT('Ctrl Pts',(1.88596913666793,1.,-0.432493038548748));
#31930=CARTESIAN_POINT('Ctrl Pts',(1.89136993975504,1.,-0.435225660963383));
#31931=CARTESIAN_POINT('Ctrl Pts',(1.89663648956466,1.,-0.437995003948244));
#31932=CARTESIAN_POINT('Ctrl Pts',(1.90180124389086,1.,-0.440807833704038));
#31933=CARTESIAN_POINT('Ctrl Pts',(1.90691756144898,1.,-0.443677556849151));
#31934=CARTESIAN_POINT('Ctrl Pts',(1.9120369998112,1.,-0.446617343485711));
#31935=CARTESIAN_POINT('Ctrl Pts',(1.91718342555755,1.,-0.449632260106662));
#31936=CARTESIAN_POINT('Ctrl Pts',(1.92235380648502,1.,-0.452719478359433));
#31937=CARTESIAN_POINT('Ctrl Pts',(1.92753067150476,1.,-0.455872005174371));
#31938=CARTESIAN_POINT('Ctrl Pts',(1.93269066517934,1.,-0.459081234547926));
#31939=CARTESIAN_POINT('Ctrl Pts',(1.93781486640821,1.,-0.462340031009057));
#31940=CARTESIAN_POINT('Ctrl Pts',(1.9428979419619,1.,-0.46564546202603));
#31941=CARTESIAN_POINT('Ctrl Pts',(1.94794381136514,1.,-0.468997482913135));
#31942=CARTESIAN_POINT('Ctrl Pts',(1.95296148278133,1.,-0.472397672264072));
#31943=CARTESIAN_POINT('Ctrl Pts',(1.95796111148177,1.,-0.475848034683176));
#31944=CARTESIAN_POINT('Ctrl Pts',(1.96294933055943,1.,-0.479349583074855));
#31945=CARTESIAN_POINT('Ctrl Pts',(1.96792703422362,1.,-0.482901662120691));
#31946=CARTESIAN_POINT('Ctrl Pts',(1.97289186263272,1.,-0.486502692907659));
#31947=CARTESIAN_POINT('Ctrl Pts',(1.97783973019229,1.,-0.490150627860953));
#31948=CARTESIAN_POINT('Ctrl Pts',(1.98276658761821,1.,-0.493843476541495));
#31949=CARTESIAN_POINT('Ctrl Pts',(1.98767044752932,1.,-0.497579909545574));
#31950=CARTESIAN_POINT('Ctrl Pts',(1.99255149126155,1.,-0.501359287727146));
#31951=CARTESIAN_POINT('Ctrl Pts',(1.99741107463572,1.,-0.505181361323026));
#31952=CARTESIAN_POINT('Ctrl Pts',(2.00225107134734,1.,-0.509046069886157));
#31953=CARTESIAN_POINT('Ctrl Pts',(2.00707309946949,1.,-0.512953306961793));
#31954=CARTESIAN_POINT('Ctrl Pts',(2.01187773939242,1.,-0.516902681728687));
#31955=CARTESIAN_POINT('Ctrl Pts',(2.01666477917286,1.,-0.520893590399371));
#31956=CARTESIAN_POINT('Ctrl Pts',(2.02143356304698,1.,-0.524925318333476));
#31957=CARTESIAN_POINT('Ctrl Pts',(2.0261832908329,1.,-0.528997127241914));
#31958=CARTESIAN_POINT('Ctrl Pts',(2.03091336214426,1.,-0.533108355132977));
#31959=CARTESIAN_POINT('Ctrl Pts',(2.03562362954037,1.,-0.537258489833262));
#31960=CARTESIAN_POINT('Ctrl Pts',(2.04031422690527,1.,-0.541447120615659));
#31961=CARTESIAN_POINT('Ctrl Pts',(2.04498544714588,1.,-0.54567390381743));
#31962=CARTESIAN_POINT('Ctrl Pts',(2.04963761077958,1.,-0.549938525150295));
#31963=CARTESIAN_POINT('Ctrl Pts',(2.05427091604413,1.,-0.554240657463906));
#31964=CARTESIAN_POINT('Ctrl Pts',(2.05888537756462,1.,-0.558579940185152));
#31965=CARTESIAN_POINT('Ctrl Pts',(2.06348090160589,1.,-0.562955993082262));
#31966=CARTESIAN_POINT('Ctrl Pts',(2.06805732997334,1.,-0.567368421181087));
#31967=CARTESIAN_POINT('Ctrl Pts',(2.07261449292824,1.,-0.571816823242603));
#31968=CARTESIAN_POINT('Ctrl Pts',(2.07715226767559,1.,-0.576300797416845));
#31969=CARTESIAN_POINT('Ctrl Pts',(2.08167059018418,1.,-0.580819952108064));
#31970=CARTESIAN_POINT('Ctrl Pts',(2.08616943727951,1.,-0.585373918991617));
#31971=CARTESIAN_POINT('Ctrl Pts',(2.09064881812129,1.,-0.589962365403406));
#31972=CARTESIAN_POINT('Ctrl Pts',(2.0951087622027,1.,-0.594585006052162));
#31973=CARTESIAN_POINT('Ctrl Pts',(2.0995493086477,1.,-0.599241616420534));
#31974=CARTESIAN_POINT('Ctrl Pts',(2.10397049886949,1.,-0.60393203073603));
#31975=CARTESIAN_POINT('Ctrl Pts',(2.1074919961518,1.,-0.607711315454876));
#31976=CARTESIAN_POINT('Ctrl Pts',(2.11012443807238,1.,-0.610560911689899));
#31977=CARTESIAN_POINT('Ctrl Pts',(2.11187554259986,1.,-0.6124673655618));
#31978=CARTESIAN_POINT('Ctrl Pts',(2.11275013067528,1.,-0.61342227326009));
#31979=CARTESIAN_POINT('',(1.7075470150345,0.,-0.383122945602001));
#31980=CARTESIAN_POINT('Origin',(0.,0.,0.));
#31981=CARTESIAN_POINT('',(1.74236521665491,1.,-0.163289472382896));
#31982=CARTESIAN_POINT('Origin',(0.,1.,0.));
#31983=CARTESIAN_POINT('',(1.74236521665491,0.,-0.163289472382896));
#31984=CARTESIAN_POINT('Ctrl Pts',(2.19890268624765,-1.,-0.0694764450219582));
#31985=CARTESIAN_POINT('Ctrl Pts',(2.19890268624765,1.,-0.0694764450219582));
#31986=CARTESIAN_POINT('Ctrl Pts',(2.19777582085423,-1.,-0.0701143536325491));
#31987=CARTESIAN_POINT('Ctrl Pts',(2.19777582085423,1.,-0.0701143536325491));
#31988=CARTESIAN_POINT('Ctrl Pts',(2.19552129484002,-1.,-0.0713863779526155));
#31989=CARTESIAN_POINT('Ctrl Pts',(2.19552129484002,1.,-0.0713863779526155));
#31990=CARTESIAN_POINT('Ctrl Pts',(2.19213712013662,-1.,-0.0732830357306726));
#31991=CARTESIAN_POINT('Ctrl Pts',(2.19213712013662,1.,-0.0732830357306726));
#31992=CARTESIAN_POINT('Ctrl Pts',(2.1876201139953,-1.,-0.0757891465836149));
#31993=CARTESIAN_POINT('Ctrl Pts',(2.1876201139953,1.,-0.0757891465836149));
#31994=CARTESIAN_POINT('Ctrl Pts',(2.18196589448887,-1.,-0.0788837727685244));
#31995=CARTESIAN_POINT('Ctrl Pts',(2.18196589448887,1.,-0.0788837727685244));
#31996=CARTESIAN_POINT('Ctrl Pts',(2.176303712113,-1.,-0.0819402680872767));
#31997=CARTESIAN_POINT('Ctrl Pts',(2.176303712113,1.,-0.0819402680872767));
#31998=CARTESIAN_POINT('Ctrl Pts',(2.17063357870952,-1.,-0.0849584620835374));
#31999=CARTESIAN_POINT('Ctrl Pts',(2.17063357870952,1.,-0.0849584620835374));
#32000=CARTESIAN_POINT('Ctrl Pts',(2.16495552645014,-1.,-0.0879381291386924));
#32001=CARTESIAN_POINT('Ctrl Pts',(2.16495552645014,1.,-0.0879381291386924));
#32002=CARTESIAN_POINT('Ctrl Pts',(2.15926961544516,-1.,-0.0908789888107267));
#32003=CARTESIAN_POINT('Ctrl Pts',(2.15926961544516,1.,-0.0908789888107267));
#32004=CARTESIAN_POINT('Ctrl Pts',(2.1535759397817,-1.,-0.0937807218867645));
#32005=CARTESIAN_POINT('Ctrl Pts',(2.1535759397817,1.,-0.0937807218867645));
#32006=CARTESIAN_POINT('Ctrl Pts',(2.14787463531795,-1.,-0.096642985230546));
#32007=CARTESIAN_POINT('Ctrl Pts',(2.14787463531795,1.,-0.096642985230546));
#32008=CARTESIAN_POINT('Ctrl Pts',(2.14216588396025,-1.,-0.0994654261990917));
#32009=CARTESIAN_POINT('Ctrl Pts',(2.14216588396025,1.,-0.0994654261990917));
#32010=CARTESIAN_POINT('Ctrl Pts',(2.13644992667165,-1.,-0.102247700556101));
#32011=CARTESIAN_POINT('Ctrl Pts',(2.13644992667165,1.,-0.102247700556101));
#32012=CARTESIAN_POINT('Ctrl Pts',(2.13072704887293,-1.,-0.10498947915274));
#32013=CARTESIAN_POINT('Ctrl Pts',(2.13072704887293,1.,-0.10498947915274));
#32014=CARTESIAN_POINT('Ctrl Pts',(2.12499752307,-1.,-0.10769043523109));
#32015=CARTESIAN_POINT('Ctrl Pts',(2.12499752307,1.,-0.10769043523109));
#32016=CARTESIAN_POINT('Ctrl Pts',(2.11926155590865,-1.,-0.110350236135025));
#32017=CARTESIAN_POINT('Ctrl Pts',(2.11926155590865,1.,-0.110350236135025));
#32018=CARTESIAN_POINT('Ctrl Pts',(2.11351924490306,-1.,-0.112968534419737));
#32019=CARTESIAN_POINT('Ctrl Pts',(2.11351924490306,1.,-0.112968534419737));
#32020=CARTESIAN_POINT('Ctrl Pts',(2.10777050261309,-1.,-0.115544957687927));
#32021=CARTESIAN_POINT('Ctrl Pts',(2.10777050261309,1.,-0.115544957687927));
#32022=CARTESIAN_POINT('Ctrl Pts',(2.102015121329,-1.,-0.118079107988356));
#32023=CARTESIAN_POINT('Ctrl Pts',(2.102015121329,1.,-0.118079107988356));
#32024=CARTESIAN_POINT('Ctrl Pts',(2.0962529286773,-1.,-0.120570567965122));
#32025=CARTESIAN_POINT('Ctrl Pts',(2.0962529286773,1.,-0.120570567965122));
#32026=CARTESIAN_POINT('Ctrl Pts',(2.09048392424825,-1.,-0.123018905621083));
#32027=CARTESIAN_POINT('Ctrl Pts',(2.09048392424825,1.,-0.123018905621083));
#32028=CARTESIAN_POINT('Ctrl Pts',(2.08470840653643,-1.,-0.125423679412062));
#32029=CARTESIAN_POINT('Ctrl Pts',(2.08470840653643,1.,-0.125423679412062));
#32030=CARTESIAN_POINT('Ctrl Pts',(2.07892715110987,-1.,-0.12778444527612));
#32031=CARTESIAN_POINT('Ctrl Pts',(2.07892715110987,1.,-0.12778444527612));
#32032=CARTESIAN_POINT('Ctrl Pts',(2.07314114713063,-1.,-0.130100748328404));
#32033=CARTESIAN_POINT('Ctrl Pts',(2.07314114713063,1.,-0.130100748328404));
#32034=CARTESIAN_POINT('Ctrl Pts',(2.06735123910326,-1.,-0.132372111547711));
#32035=CARTESIAN_POINT('Ctrl Pts',(2.06735123910326,1.,-0.132372111547711));
#32036=CARTESIAN_POINT('Ctrl Pts',(2.06155781517842,-1.,-0.134598026192106));
#32037=CARTESIAN_POINT('Ctrl Pts',(2.06155781517842,1.,-0.134598026192106));
#32038=CARTESIAN_POINT('Ctrl Pts',(2.05576044414264,-1.,-0.136777941218044));
#32039=CARTESIAN_POINT('Ctrl Pts',(2.05576044414264,1.,-0.136777941218044));
#32040=CARTESIAN_POINT('Ctrl Pts',(2.04995762001328,-1.,-0.138911255368966));
#32041=CARTESIAN_POINT('Ctrl Pts',(2.04995762001328,1.,-0.138911255368966));
#32042=CARTESIAN_POINT('Ctrl Pts',(2.04414757947916,-1.,-0.140997332152546));
#32043=CARTESIAN_POINT('Ctrl Pts',(2.04414757947916,1.,-0.140997332152546));
#32044=CARTESIAN_POINT('Ctrl Pts',(2.03832911025912,-1.,-0.143035515058209));
#32045=CARTESIAN_POINT('Ctrl Pts',(2.03832911025912,1.,-0.143035515058209));
#32046=CARTESIAN_POINT('Ctrl Pts',(2.03250223739942,-1.,-0.145025140186058));
#32047=CARTESIAN_POINT('Ctrl Pts',(2.03250223739942,1.,-0.145025140186058));
#32048=CARTESIAN_POINT('Ctrl Pts',(2.02666926182017,-1.,-0.146965557332583));
#32049=CARTESIAN_POINT('Ctrl Pts',(2.02666926182017,1.,-0.146965557332583));
#32050=CARTESIAN_POINT('Ctrl Pts',(2.02083464969894,-1.,-0.148856124775337));
#32051=CARTESIAN_POINT('Ctrl Pts',(2.02083464969894,1.,-0.148856124775337));
#32052=CARTESIAN_POINT('Ctrl Pts',(2.01500291940238,-1.,-0.150696157673078));
#32053=CARTESIAN_POINT('Ctrl Pts',(2.01500291940238,1.,-0.150696157673078));
#32054=CARTESIAN_POINT('Ctrl Pts',(2.00917680318424,-1.,-0.15248488362145));
#32055=CARTESIAN_POINT('Ctrl Pts',(2.00917680318424,1.,-0.15248488362145));
#32056=CARTESIAN_POINT('Ctrl Pts',(2.00335565310543,-1.,-0.154221403049722));
#32057=CARTESIAN_POINT('Ctrl Pts',(2.00335565310543,1.,-0.154221403049722));
#32058=CARTESIAN_POINT('Ctrl Pts',(1.99753284771497,-1.,-0.155904629548784));
#32059=CARTESIAN_POINT('Ctrl Pts',(1.99753284771497,1.,-0.155904629548784));
#32060=CARTESIAN_POINT('Ctrl Pts',(1.99169810931908,-1.,-0.157533331459227));
#32061=CARTESIAN_POINT('Ctrl Pts',(1.99169810931908,1.,-0.157533331459227));
#32062=CARTESIAN_POINT('Ctrl Pts',(1.98584238283292,-1.,-0.159106226437299));
#32063=CARTESIAN_POINT('Ctrl Pts',(1.98584238283292,1.,-0.159106226437299));
#32064=CARTESIAN_POINT('Ctrl Pts',(1.97996195437559,-1.,-0.160622060784611));
#32065=CARTESIAN_POINT('Ctrl Pts',(1.97996195437559,1.,-0.160622060784611));
#32066=CARTESIAN_POINT('Ctrl Pts',(1.97406280235188,-1.,-0.162079693556289));
#32067=CARTESIAN_POINT('Ctrl Pts',(1.97406280235188,1.,-0.162079693556289));
#32068=CARTESIAN_POINT('Ctrl Pts',(1.96816512677967,-1.,-0.163478185457734));
#32069=CARTESIAN_POINT('Ctrl Pts',(1.96816512677967,1.,-0.163478185457734));
#32070=CARTESIAN_POINT('Ctrl Pts',(1.96229379940136,-1.,-0.164816568920269));
#32071=CARTESIAN_POINT('Ctrl Pts',(1.96229379940136,1.,-0.164816568920269));
#32072=CARTESIAN_POINT('Ctrl Pts',(1.9564675971873,-1.,-0.166093592002813));
#32073=CARTESIAN_POINT('Ctrl Pts',(1.9564675971873,1.,-0.166093592002813));
#32074=CARTESIAN_POINT('Ctrl Pts',(1.95069027794294,-1.,-0.167307501784476));
#32075=CARTESIAN_POINT('Ctrl Pts',(1.95069027794294,1.,-0.167307501784476));
#32076=CARTESIAN_POINT('Ctrl Pts',(1.94493757756931,-1.,-0.168455741607556));
#32077=CARTESIAN_POINT('Ctrl Pts',(1.94493757756931,1.,-0.168455741607556));
#32078=CARTESIAN_POINT('Ctrl Pts',(1.93915639211581,-1.,-0.169534904817491));
#32079=CARTESIAN_POINT('Ctrl Pts',(1.93915639211581,1.,-0.169534904817491));
#32080=CARTESIAN_POINT('Ctrl Pts',(1.93329183155539,-1.,-0.170541253116202));
#32081=CARTESIAN_POINT('Ctrl Pts',(1.93329183155539,1.,-0.170541253116202));
#32082=CARTESIAN_POINT('Ctrl Pts',(1.92731093582036,-1.,-0.171471191532988));
#32083=CARTESIAN_POINT('Ctrl Pts',(1.92731093582036,1.,-0.171471191532988));
#32084=CARTESIAN_POINT('Ctrl Pts',(1.9212233439798,-1.,-0.172321621259514));
#32085=CARTESIAN_POINT('Ctrl Pts',(1.9212233439798,1.,-0.172321621259514));
#32086=CARTESIAN_POINT('Ctrl Pts',(1.91511429159527,-1.,-0.173090695383496));
#32087=CARTESIAN_POINT('Ctrl Pts',(1.91511429159527,1.,-0.173090695383496));
#32088=CARTESIAN_POINT('Ctrl Pts',(1.90911693975267,-1.,-0.173776635257817));
#32089=CARTESIAN_POINT('Ctrl Pts',(1.90911693975267,1.,-0.173776635257817));
#32090=CARTESIAN_POINT('Ctrl Pts',(1.90335253862834,-1.,-0.174375518661085));
#32091=CARTESIAN_POINT('Ctrl Pts',(1.90335253862834,1.,-0.174375518661085));
#32092=CARTESIAN_POINT('Ctrl Pts',(1.89788101117132,-1.,-0.174879405091263));
#32093=CARTESIAN_POINT('Ctrl Pts',(1.89788101117132,1.,-0.174879405091263));
#32094=CARTESIAN_POINT('Ctrl Pts',(1.892646301985,-1.,-0.175274276190844));
#32095=CARTESIAN_POINT('Ctrl Pts',(1.892646301985,1.,-0.175274276190844));
#32096=CARTESIAN_POINT('Ctrl Pts',(1.88742606273259,-1.,-0.175538155840648));
#32097=CARTESIAN_POINT('Ctrl Pts',(1.88742606273259,1.,-0.175538155840648));
#32098=CARTESIAN_POINT('Ctrl Pts',(1.88188663145367,-1.,-0.175644148889699));
#32099=CARTESIAN_POINT('Ctrl Pts',(1.88188663145367,1.,-0.175644148889699));
#32100=CARTESIAN_POINT('Ctrl Pts',(1.87563767773588,-1.,-0.175563480746485));
#32101=CARTESIAN_POINT('Ctrl Pts',(1.87563767773588,1.,-0.175563480746485));
#32102=CARTESIAN_POINT('Ctrl Pts',(1.86828349694799,-1.,-0.175268337590758));
#32103=CARTESIAN_POINT('Ctrl Pts',(1.86828349694799,1.,-0.175268337590758));
#32104=CARTESIAN_POINT('Ctrl Pts',(1.85948367088837,-1.,-0.17473525927603));
#32105=CARTESIAN_POINT('Ctrl Pts',(1.85948367088837,1.,-0.17473525927603));
#32106=CARTESIAN_POINT('Ctrl Pts',(1.8489811319852,-1.,-0.173946627587732));
#32107=CARTESIAN_POINT('Ctrl Pts',(1.8489811319852,1.,-0.173946627587732));
#32108=CARTESIAN_POINT('Ctrl Pts',(1.83658380527692,-1.,-0.1728894428919));
#32109=CARTESIAN_POINT('Ctrl Pts',(1.83658380527692,1.,-0.1728894428919));
#32110=CARTESIAN_POINT('Ctrl Pts',(1.82215766811545,-1.,-0.171554770204119));
#32111=CARTESIAN_POINT('Ctrl Pts',(1.82215766811545,1.,-0.171554770204119));
#32112=CARTESIAN_POINT('Ctrl Pts',(1.80561530629706,-1.,-0.169936923904608));
#32113=CARTESIAN_POINT('Ctrl Pts',(1.80561530629706,1.,-0.169936923904608));
#32114=CARTESIAN_POINT('Ctrl Pts',(1.7869064998507,-1.,-0.168032772805197));
#32115=CARTESIAN_POINT('Ctrl Pts',(1.7869064998507,1.,-0.168032772805197));
#32116=CARTESIAN_POINT('Ctrl Pts',(1.77018771684844,-1.,-0.1662793551464));
#32117=CARTESIAN_POINT('Ctrl Pts',(1.77018771684844,1.,-0.1662793551464));
#32118=CARTESIAN_POINT('Ctrl Pts',(1.75666056638427,-1.,-0.164834765707159));
#32119=CARTESIAN_POINT('Ctrl Pts',(1.75666056638427,1.,-0.164834765707159));
#32120=CARTESIAN_POINT('Ctrl Pts',(1.7472034950333,-1.,-0.163814161002002));
#32121=CARTESIAN_POINT('Ctrl Pts',(1.7472034950333,1.,-0.163814161002002));
#32122=CARTESIAN_POINT('Ctrl Pts',(1.74236521665491,-1.,-0.163289472382896));
#32123=CARTESIAN_POINT('Ctrl Pts',(1.74236521665491,1.,-0.163289472382896));
#32124=CARTESIAN_POINT('',(2.19890268624765,1.,-0.0694764450219582));
#32125=CARTESIAN_POINT('Ctrl Pts',(2.19890268624765,1.,-0.0694764450219582));
#32126=CARTESIAN_POINT('Ctrl Pts',(2.19777582085423,1.,-0.0701143536325491));
#32127=CARTESIAN_POINT('Ctrl Pts',(2.19552129484002,1.,-0.0713863779526155));
#32128=CARTESIAN_POINT('Ctrl Pts',(2.19213712013662,1.,-0.0732830357306726));
#32129=CARTESIAN_POINT('Ctrl Pts',(2.1876201139953,1.,-0.0757891465836149));
#32130=CARTESIAN_POINT('Ctrl Pts',(2.18196589448887,1.,-0.0788837727685244));
#32131=CARTESIAN_POINT('Ctrl Pts',(2.176303712113,1.,-0.0819402680872767));
#32132=CARTESIAN_POINT('Ctrl Pts',(2.17063357870952,1.,-0.0849584620835374));
#32133=CARTESIAN_POINT('Ctrl Pts',(2.16495552645014,1.,-0.0879381291386924));
#32134=CARTESIAN_POINT('Ctrl Pts',(2.15926961544516,1.,-0.0908789888107267));
#32135=CARTESIAN_POINT('Ctrl Pts',(2.1535759397817,1.,-0.0937807218867645));
#32136=CARTESIAN_POINT('Ctrl Pts',(2.14787463531795,1.,-0.096642985230546));
#32137=CARTESIAN_POINT('Ctrl Pts',(2.14216588396025,1.,-0.0994654261990917));
#32138=CARTESIAN_POINT('Ctrl Pts',(2.13644992667165,1.,-0.102247700556101));
#32139=CARTESIAN_POINT('Ctrl Pts',(2.13072704887293,1.,-0.10498947915274));
#32140=CARTESIAN_POINT('Ctrl Pts',(2.12499752307,1.,-0.10769043523109));
#32141=CARTESIAN_POINT('Ctrl Pts',(2.11926155590865,1.,-0.110350236135025));
#32142=CARTESIAN_POINT('Ctrl Pts',(2.11351924490306,1.,-0.112968534419737));
#32143=CARTESIAN_POINT('Ctrl Pts',(2.10777050261309,1.,-0.115544957687927));
#32144=CARTESIAN_POINT('Ctrl Pts',(2.102015121329,1.,-0.118079107988356));
#32145=CARTESIAN_POINT('Ctrl Pts',(2.0962529286773,1.,-0.120570567965122));
#32146=CARTESIAN_POINT('Ctrl Pts',(2.09048392424825,1.,-0.123018905621083));
#32147=CARTESIAN_POINT('Ctrl Pts',(2.08470840653643,1.,-0.125423679412062));
#32148=CARTESIAN_POINT('Ctrl Pts',(2.07892715110987,1.,-0.12778444527612));
#32149=CARTESIAN_POINT('Ctrl Pts',(2.07314114713063,1.,-0.130100748328404));
#32150=CARTESIAN_POINT('Ctrl Pts',(2.06735123910326,1.,-0.132372111547711));
#32151=CARTESIAN_POINT('Ctrl Pts',(2.06155781517842,1.,-0.134598026192106));
#32152=CARTESIAN_POINT('Ctrl Pts',(2.05576044414264,1.,-0.136777941218044));
#32153=CARTESIAN_POINT('Ctrl Pts',(2.04995762001328,1.,-0.138911255368966));
#32154=CARTESIAN_POINT('Ctrl Pts',(2.04414757947916,1.,-0.140997332152546));
#32155=CARTESIAN_POINT('Ctrl Pts',(2.03832911025912,1.,-0.143035515058209));
#32156=CARTESIAN_POINT('Ctrl Pts',(2.03250223739942,1.,-0.145025140186058));
#32157=CARTESIAN_POINT('Ctrl Pts',(2.02666926182017,1.,-0.146965557332583));
#32158=CARTESIAN_POINT('Ctrl Pts',(2.02083464969894,1.,-0.148856124775337));
#32159=CARTESIAN_POINT('Ctrl Pts',(2.01500291940238,1.,-0.150696157673078));
#32160=CARTESIAN_POINT('Ctrl Pts',(2.00917680318424,1.,-0.15248488362145));
#32161=CARTESIAN_POINT('Ctrl Pts',(2.00335565310543,1.,-0.154221403049722));
#32162=CARTESIAN_POINT('Ctrl Pts',(1.99753284771497,1.,-0.155904629548784));
#32163=CARTESIAN_POINT('Ctrl Pts',(1.99169810931908,1.,-0.157533331459227));
#32164=CARTESIAN_POINT('Ctrl Pts',(1.98584238283292,1.,-0.159106226437299));
#32165=CARTESIAN_POINT('Ctrl Pts',(1.97996195437559,1.,-0.160622060784611));
#32166=CARTESIAN_POINT('Ctrl Pts',(1.97406280235188,1.,-0.162079693556289));
#32167=CARTESIAN_POINT('Ctrl Pts',(1.96816512677967,1.,-0.163478185457734));
#32168=CARTESIAN_POINT('Ctrl Pts',(1.96229379940136,1.,-0.164816568920269));
#32169=CARTESIAN_POINT('Ctrl Pts',(1.9564675971873,1.,-0.166093592002813));
#32170=CARTESIAN_POINT('Ctrl Pts',(1.95069027794294,1.,-0.167307501784476));
#32171=CARTESIAN_POINT('Ctrl Pts',(1.94493757756931,1.,-0.168455741607556));
#32172=CARTESIAN_POINT('Ctrl Pts',(1.93915639211581,1.,-0.169534904817491));
#32173=CARTESIAN_POINT('Ctrl Pts',(1.93329183155539,1.,-0.170541253116202));
#32174=CARTESIAN_POINT('Ctrl Pts',(1.92731093582036,1.,-0.171471191532988));
#32175=CARTESIAN_POINT('Ctrl Pts',(1.9212233439798,1.,-0.172321621259514));
#32176=CARTESIAN_POINT('Ctrl Pts',(1.91511429159527,1.,-0.173090695383496));
#32177=CARTESIAN_POINT('Ctrl Pts',(1.90911693975267,1.,-0.173776635257817));
#32178=CARTESIAN_POINT('Ctrl Pts',(1.90335253862834,1.,-0.174375518661085));
#32179=CARTESIAN_POINT('Ctrl Pts',(1.89788101117132,1.,-0.174879405091263));
#32180=CARTESIAN_POINT('Ctrl Pts',(1.892646301985,1.,-0.175274276190844));
#32181=CARTESIAN_POINT('Ctrl Pts',(1.88742606273259,1.,-0.175538155840648));
#32182=CARTESIAN_POINT('Ctrl Pts',(1.88188663145367,1.,-0.175644148889699));
#32183=CARTESIAN_POINT('Ctrl Pts',(1.87563767773588,1.,-0.175563480746485));
#32184=CARTESIAN_POINT('Ctrl Pts',(1.86828349694799,1.,-0.175268337590758));
#32185=CARTESIAN_POINT('Ctrl Pts',(1.85948367088837,1.,-0.17473525927603));
#32186=CARTESIAN_POINT('Ctrl Pts',(1.8489811319852,1.,-0.173946627587732));
#32187=CARTESIAN_POINT('Ctrl Pts',(1.83658380527692,1.,-0.1728894428919));
#32188=CARTESIAN_POINT('Ctrl Pts',(1.82215766811545,1.,-0.171554770204119));
#32189=CARTESIAN_POINT('Ctrl Pts',(1.80561530629706,1.,-0.169936923904608));
#32190=CARTESIAN_POINT('Ctrl Pts',(1.7869064998507,1.,-0.168032772805197));
#32191=CARTESIAN_POINT('Ctrl Pts',(1.77018771684844,1.,-0.1662793551464));
#32192=CARTESIAN_POINT('Ctrl Pts',(1.75666056638427,1.,-0.164834765707159));
#32193=CARTESIAN_POINT('Ctrl Pts',(1.7472034950333,1.,-0.163814161002002));
#32194=CARTESIAN_POINT('Ctrl Pts',(1.74236521665491,1.,-0.163289472382896));
#32195=CARTESIAN_POINT('',(2.19890268624765,0.,-0.0694764450219582));
#32196=CARTESIAN_POINT('Origin',(2.19890268624765,0.,0.0694764450219582));
#32197=CARTESIAN_POINT('',(2.19890268624765,1.,0.0694764450219582));
#32198=CARTESIAN_POINT('',(2.19890268624765,1.,-0.0694764450219582));
#32199=CARTESIAN_POINT('',(2.19890268624765,0.,0.0694764450219582));
#32200=CARTESIAN_POINT('Ctrl Pts',(1.74236521665491,-1.,0.163289472382896));
#32201=CARTESIAN_POINT('Ctrl Pts',(1.74236521665491,1.,0.163289472382896));
#32202=CARTESIAN_POINT('Ctrl Pts',(1.74720349503904,-1.,0.163814161002474));
#32203=CARTESIAN_POINT('Ctrl Pts',(1.74720349503904,1.,0.163814161002474));
#32204=CARTESIAN_POINT('Ctrl Pts',(1.75666056640041,-1.,0.164834765708484));
#32205=CARTESIAN_POINT('Ctrl Pts',(1.75666056640041,1.,0.164834765708484));
#32206=CARTESIAN_POINT('Ctrl Pts',(1.77018771687692,-1.,0.166279355148738));
#32207=CARTESIAN_POINT('Ctrl Pts',(1.77018771687692,1.,0.166279355148738));
#32208=CARTESIAN_POINT('Ctrl Pts',(1.78690649988931,-1.,0.16803277280837));
#32209=CARTESIAN_POINT('Ctrl Pts',(1.78690649988931,1.,0.16803277280837));
#32210=CARTESIAN_POINT('Ctrl Pts',(1.80561530633924,-1.,0.169936923908078));
#32211=CARTESIAN_POINT('Ctrl Pts',(1.80561530633924,1.,0.169936923908078));
#32212=CARTESIAN_POINT('Ctrl Pts',(1.82215766815414,-1.,0.171554770207306));
#32213=CARTESIAN_POINT('Ctrl Pts',(1.82215766815414,1.,0.171554770207306));
#32214=CARTESIAN_POINT('Ctrl Pts',(1.83658380530747,-1.,0.17288944289442));
#32215=CARTESIAN_POINT('Ctrl Pts',(1.83658380530747,1.,0.17288944289442));
#32216=CARTESIAN_POINT('Ctrl Pts',(1.84898113200543,-1.,0.173946627589401));
#32217=CARTESIAN_POINT('Ctrl Pts',(1.84898113200543,1.,0.173946627589401));
#32218=CARTESIAN_POINT('Ctrl Pts',(1.85948367089838,-1.,0.174735259276856));
#32219=CARTESIAN_POINT('Ctrl Pts',(1.85948367089838,1.,0.174735259276856));
#32220=CARTESIAN_POINT('Ctrl Pts',(1.86828349694972,-1.,0.1752683375909));
#32221=CARTESIAN_POINT('Ctrl Pts',(1.86828349694972,1.,0.1752683375909));
#32222=CARTESIAN_POINT('Ctrl Pts',(1.87563767773249,-1.,0.175563480746205));
#32223=CARTESIAN_POINT('Ctrl Pts',(1.87563767773249,1.,0.175563480746205));
#32224=CARTESIAN_POINT('Ctrl Pts',(1.88188663144846,-1.,0.175644148889271));
#32225=CARTESIAN_POINT('Ctrl Pts',(1.88188663144846,1.,0.175644148889271));
#32226=CARTESIAN_POINT('Ctrl Pts',(1.88742606272818,-1.,0.175538155840286));
#32227=CARTESIAN_POINT('Ctrl Pts',(1.88742606272818,1.,0.175538155840286));
#32228=CARTESIAN_POINT('Ctrl Pts',(1.89264630198279,-1.,0.175274276190664));
#32229=CARTESIAN_POINT('Ctrl Pts',(1.89264630198279,1.,0.175274276190664));
#32230=CARTESIAN_POINT('Ctrl Pts',(1.89788101117148,-1.,0.174879405091277));
#32231=CARTESIAN_POINT('Ctrl Pts',(1.89788101117148,1.,0.174879405091277));
#32232=CARTESIAN_POINT('Ctrl Pts',(1.90335253863003,-1.,0.174375518661222));
#32233=CARTESIAN_POINT('Ctrl Pts',(1.90335253863003,1.,0.174375518661222));
#32234=CARTESIAN_POINT('Ctrl Pts',(1.90911693975475,-1.,0.173776635257983));
#32235=CARTESIAN_POINT('Ctrl Pts',(1.90911693975475,1.,0.173776635257983));
#32236=CARTESIAN_POINT('Ctrl Pts',(1.91511429159681,-1.,0.173090695383619));
#32237=CARTESIAN_POINT('Ctrl Pts',(1.91511429159681,1.,0.173090695383619));
#32238=CARTESIAN_POINT('Ctrl Pts',(1.92122334398034,-1.,0.172321621259556));
#32239=CARTESIAN_POINT('Ctrl Pts',(1.92122334398034,1.,0.172321621259556));
#32240=CARTESIAN_POINT('Ctrl Pts',(1.92731093582,-1.,0.17147119153296));
#32241=CARTESIAN_POINT('Ctrl Pts',(1.92731093582,1.,0.17147119153296));
#32242=CARTESIAN_POINT('Ctrl Pts',(1.93329183155455,-1.,0.170541253116136));
#32243=CARTESIAN_POINT('Ctrl Pts',(1.93329183155455,1.,0.170541253116136));
#32244=CARTESIAN_POINT('Ctrl Pts',(1.93915639211497,-1.,0.169534904817425));
#32245=CARTESIAN_POINT('Ctrl Pts',(1.93915639211497,1.,0.169534904817425));
#32246=CARTESIAN_POINT('Ctrl Pts',(1.94493757756879,-1.,0.168455741607515));
#32247=CARTESIAN_POINT('Ctrl Pts',(1.94493757756879,1.,0.168455741607515));
#32248=CARTESIAN_POINT('Ctrl Pts',(1.95069027794286,-1.,0.167307501784469));
#32249=CARTESIAN_POINT('Ctrl Pts',(1.95069027794286,1.,0.167307501784469));
#32250=CARTESIAN_POINT('Ctrl Pts',(1.95646759718755,-1.,0.166093592002832));
#32251=CARTESIAN_POINT('Ctrl Pts',(1.95646759718755,1.,0.166093592002832));
#32252=CARTESIAN_POINT('Ctrl Pts',(1.96229379940174,-1.,0.1648165689203));
#32253=CARTESIAN_POINT('Ctrl Pts',(1.96229379940174,1.,0.1648165689203));
#32254=CARTESIAN_POINT('Ctrl Pts',(1.96816512678,-1.,0.16347818545776));
#32255=CARTESIAN_POINT('Ctrl Pts',(1.96816512678,1.,0.16347818545776));
#32256=CARTESIAN_POINT('Ctrl Pts',(1.97406280235204,-1.,0.162079693556302));
#32257=CARTESIAN_POINT('Ctrl Pts',(1.97406280235204,1.,0.162079693556302));
#32258=CARTESIAN_POINT('Ctrl Pts',(1.97996195437557,-1.,0.16062206078461));
#32259=CARTESIAN_POINT('Ctrl Pts',(1.97996195437557,1.,0.16062206078461));
#32260=CARTESIAN_POINT('Ctrl Pts',(1.98584238283279,-1.,0.159106226437288));
#32261=CARTESIAN_POINT('Ctrl Pts',(1.98584238283279,1.,0.159106226437288));
#32262=CARTESIAN_POINT('Ctrl Pts',(1.99169810931893,-1.,0.157533331459215));
#32263=CARTESIAN_POINT('Ctrl Pts',(1.99169810931893,1.,0.157533331459215));
#32264=CARTESIAN_POINT('Ctrl Pts',(1.99753284771487,-1.,0.155904629548774));
#32265=CARTESIAN_POINT('Ctrl Pts',(1.99753284771487,1.,0.155904629548774));
#32266=CARTESIAN_POINT('Ctrl Pts',(2.00335565310539,-1.,0.154221403049719));
#32267=CARTESIAN_POINT('Ctrl Pts',(2.00335565310539,1.,0.154221403049719));
#32268=CARTESIAN_POINT('Ctrl Pts',(2.00917680318426,-1.,0.152484883621452));
#32269=CARTESIAN_POINT('Ctrl Pts',(2.00917680318426,1.,0.152484883621452));
#32270=CARTESIAN_POINT('Ctrl Pts',(2.01500291940243,-1.,0.150696157673084));
#32271=CARTESIAN_POINT('Ctrl Pts',(2.01500291940243,1.,0.150696157673084));
#32272=CARTESIAN_POINT('Ctrl Pts',(2.02083464969897,-1.,0.148856124775342));
#32273=CARTESIAN_POINT('Ctrl Pts',(2.02083464969897,1.,0.148856124775342));
#32274=CARTESIAN_POINT('Ctrl Pts',(2.02666926182017,-1.,0.146965557332586));
#32275=CARTESIAN_POINT('Ctrl Pts',(2.02666926182017,1.,0.146965557332586));
#32276=CARTESIAN_POINT('Ctrl Pts',(2.03250223739941,-1.,0.145025140186058));
#32277=CARTESIAN_POINT('Ctrl Pts',(2.03250223739941,1.,0.145025140186058));
#32278=CARTESIAN_POINT('Ctrl Pts',(2.03832911025913,-1.,0.143035515058208));
#32279=CARTESIAN_POINT('Ctrl Pts',(2.03832911025913,1.,0.143035515058208));
#32280=CARTESIAN_POINT('Ctrl Pts',(2.04414757947919,-1.,0.140997332152545));
#32281=CARTESIAN_POINT('Ctrl Pts',(2.04414757947919,1.,0.140997332152545));
#32282=CARTESIAN_POINT('Ctrl Pts',(2.04995762001333,-1.,0.138911255368966));
#32283=CARTESIAN_POINT('Ctrl Pts',(2.04995762001333,1.,0.138911255368966));
#32284=CARTESIAN_POINT('Ctrl Pts',(2.0557604441427,-1.,0.136777941218044));
#32285=CARTESIAN_POINT('Ctrl Pts',(2.0557604441427,1.,0.136777941218044));
#32286=CARTESIAN_POINT('Ctrl Pts',(2.06155781517844,-1.,0.134598026192107));
#32287=CARTESIAN_POINT('Ctrl Pts',(2.06155781517844,1.,0.134598026192107));
#32288=CARTESIAN_POINT('Ctrl Pts',(2.06735123910319,-1.,0.132372111547709));
#32289=CARTESIAN_POINT('Ctrl Pts',(2.06735123910319,1.,0.132372111547709));
#32290=CARTESIAN_POINT('Ctrl Pts',(2.07314114713047,-1.,0.1301007483284));
#32291=CARTESIAN_POINT('Ctrl Pts',(2.07314114713047,1.,0.1301007483284));
#32292=CARTESIAN_POINT('Ctrl Pts',(2.07892715110967,-1.,0.127784445276116));
#32293=CARTESIAN_POINT('Ctrl Pts',(2.07892715110967,1.,0.127784445276116));
#32294=CARTESIAN_POINT('Ctrl Pts',(2.08470840653628,-1.,0.125423679412058));
#32295=CARTESIAN_POINT('Ctrl Pts',(2.08470840653628,1.,0.125423679412058));
#32296=CARTESIAN_POINT('Ctrl Pts',(2.09048392424826,-1.,0.123018905621083));
#32297=CARTESIAN_POINT('Ctrl Pts',(2.09048392424826,1.,0.123018905621083));
#32298=CARTESIAN_POINT('Ctrl Pts',(2.09625292867756,-1.,0.120570567965129));
#32299=CARTESIAN_POINT('Ctrl Pts',(2.09625292867756,1.,0.120570567965129));
#32300=CARTESIAN_POINT('Ctrl Pts',(2.10201512132945,-1.,0.118079107988368));
#32301=CARTESIAN_POINT('Ctrl Pts',(2.10201512132945,1.,0.118079107988368));
#32302=CARTESIAN_POINT('Ctrl Pts',(2.10777050261359,-1.,0.11554495768794));
#32303=CARTESIAN_POINT('Ctrl Pts',(2.10777050261359,1.,0.11554495768794));
#32304=CARTESIAN_POINT('Ctrl Pts',(2.11351924490335,-1.,0.112968534419746));
#32305=CARTESIAN_POINT('Ctrl Pts',(2.11351924490335,1.,0.112968534419746));
#32306=CARTESIAN_POINT('Ctrl Pts',(2.11926155590849,-1.,0.11035023613502));
#32307=CARTESIAN_POINT('Ctrl Pts',(2.11926155590849,1.,0.11035023613502));
#32308=CARTESIAN_POINT('Ctrl Pts',(2.12499752306927,-1.,0.107690435231068));
#32309=CARTESIAN_POINT('Ctrl Pts',(2.12499752306927,1.,0.107690435231068));
#32310=CARTESIAN_POINT('Ctrl Pts',(2.1307270488718,-1.,0.104989479152703));
#32311=CARTESIAN_POINT('Ctrl Pts',(2.1307270488718,1.,0.104989479152703));
#32312=CARTESIAN_POINT('Ctrl Pts',(2.13644992667052,-1.,0.102247700556063));
#32313=CARTESIAN_POINT('Ctrl Pts',(2.13644992667052,1.,0.102247700556063));
#32314=CARTESIAN_POINT('Ctrl Pts',(2.14216588395974,-1.,0.0994654261990741));
#32315=CARTESIAN_POINT('Ctrl Pts',(2.14216588395974,1.,0.0994654261990741));
#32316=CARTESIAN_POINT('Ctrl Pts',(2.14787463531864,-1.,0.0966429852305688));
#32317=CARTESIAN_POINT('Ctrl Pts',(2.14787463531864,1.,0.0966429852305688));
#32318=CARTESIAN_POINT('Ctrl Pts',(2.15357593978377,-1.,0.0937807218868344));
#32319=CARTESIAN_POINT('Ctrl Pts',(2.15357593978377,1.,0.0937807218868344));
#32320=CARTESIAN_POINT('Ctrl Pts',(2.15926961544808,-1.,0.0908789888108265));
#32321=CARTESIAN_POINT('Ctrl Pts',(2.15926961544808,1.,0.0908789888108265));
#32322=CARTESIAN_POINT('Ctrl Pts',(2.16495552645275,-1.,0.0879381291387821));
#32323=CARTESIAN_POINT('Ctrl Pts',(2.16495552645275,1.,0.0879381291387821));
#32324=CARTESIAN_POINT('Ctrl Pts',(2.17063357871031,-1.,0.0849584620835642));
#32325=CARTESIAN_POINT('Ctrl Pts',(2.17063357871031,1.,0.0849584620835642));
#32326=CARTESIAN_POINT('Ctrl Pts',(2.1763037121106,-1.,0.0819402680871938));
#32327=CARTESIAN_POINT('Ctrl Pts',(2.1763037121106,1.,0.0819402680871938));
#32328=CARTESIAN_POINT('Ctrl Pts',(2.18196589448304,-1.,0.0788837727683226));
#32329=CARTESIAN_POINT('Ctrl Pts',(2.18196589448304,1.,0.0788837727683226));
#32330=CARTESIAN_POINT('Ctrl Pts',(2.1876201139874,-1.,0.075789146583341));
#32331=CARTESIAN_POINT('Ctrl Pts',(2.1876201139874,1.,0.075789146583341));
#32332=CARTESIAN_POINT('Ctrl Pts',(2.19213712012956,-1.,0.0732830357304275));
#32333=CARTESIAN_POINT('Ctrl Pts',(2.19213712012956,1.,0.0732830357304275));
#32334=CARTESIAN_POINT('Ctrl Pts',(2.19552129483562,-1.,0.0713863779524626));
#32335=CARTESIAN_POINT('Ctrl Pts',(2.19552129483562,1.,0.0713863779524626));
#32336=CARTESIAN_POINT('Ctrl Pts',(2.19777582085261,-1.,0.0701143536324925));
#32337=CARTESIAN_POINT('Ctrl Pts',(2.19777582085261,1.,0.0701143536324925));
#32338=CARTESIAN_POINT('Ctrl Pts',(2.19890268624765,-1.,0.0694764450219582));
#32339=CARTESIAN_POINT('Ctrl Pts',(2.19890268624765,1.,0.0694764450219582));
#32340=CARTESIAN_POINT('',(1.74236521665491,1.,0.163289472382896));
#32341=CARTESIAN_POINT('Ctrl Pts',(1.74236521665491,1.,0.163289472382896));
#32342=CARTESIAN_POINT('Ctrl Pts',(1.74720349503904,1.,0.163814161002474));
#32343=CARTESIAN_POINT('Ctrl Pts',(1.75666056640041,1.,0.164834765708484));
#32344=CARTESIAN_POINT('Ctrl Pts',(1.77018771687692,1.,0.166279355148738));
#32345=CARTESIAN_POINT('Ctrl Pts',(1.78690649988931,1.,0.16803277280837));
#32346=CARTESIAN_POINT('Ctrl Pts',(1.80561530633924,1.,0.169936923908078));
#32347=CARTESIAN_POINT('Ctrl Pts',(1.82215766815414,1.,0.171554770207306));
#32348=CARTESIAN_POINT('Ctrl Pts',(1.83658380530747,1.,0.17288944289442));
#32349=CARTESIAN_POINT('Ctrl Pts',(1.84898113200543,1.,0.173946627589401));
#32350=CARTESIAN_POINT('Ctrl Pts',(1.85948367089838,1.,0.174735259276856));
#32351=CARTESIAN_POINT('Ctrl Pts',(1.86828349694972,1.,0.1752683375909));
#32352=CARTESIAN_POINT('Ctrl Pts',(1.87563767773249,1.,0.175563480746205));
#32353=CARTESIAN_POINT('Ctrl Pts',(1.88188663144846,1.,0.175644148889271));
#32354=CARTESIAN_POINT('Ctrl Pts',(1.88742606272818,1.,0.175538155840286));
#32355=CARTESIAN_POINT('Ctrl Pts',(1.89264630198279,1.,0.175274276190664));
#32356=CARTESIAN_POINT('Ctrl Pts',(1.89788101117148,1.,0.174879405091277));
#32357=CARTESIAN_POINT('Ctrl Pts',(1.90335253863003,1.,0.174375518661222));
#32358=CARTESIAN_POINT('Ctrl Pts',(1.90911693975475,1.,0.173776635257983));
#32359=CARTESIAN_POINT('Ctrl Pts',(1.91511429159681,1.,0.173090695383619));
#32360=CARTESIAN_POINT('Ctrl Pts',(1.92122334398034,1.,0.172321621259556));
#32361=CARTESIAN_POINT('Ctrl Pts',(1.92731093582,1.,0.17147119153296));
#32362=CARTESIAN_POINT('Ctrl Pts',(1.93329183155455,1.,0.170541253116136));
#32363=CARTESIAN_POINT('Ctrl Pts',(1.93915639211497,1.,0.169534904817425));
#32364=CARTESIAN_POINT('Ctrl Pts',(1.94493757756879,1.,0.168455741607515));
#32365=CARTESIAN_POINT('Ctrl Pts',(1.95069027794286,1.,0.167307501784469));
#32366=CARTESIAN_POINT('Ctrl Pts',(1.95646759718755,1.,0.166093592002832));
#32367=CARTESIAN_POINT('Ctrl Pts',(1.96229379940174,1.,0.1648165689203));
#32368=CARTESIAN_POINT('Ctrl Pts',(1.96816512678,1.,0.16347818545776));
#32369=CARTESIAN_POINT('Ctrl Pts',(1.97406280235204,1.,0.162079693556302));
#32370=CARTESIAN_POINT('Ctrl Pts',(1.97996195437557,1.,0.16062206078461));
#32371=CARTESIAN_POINT('Ctrl Pts',(1.98584238283279,1.,0.159106226437288));
#32372=CARTESIAN_POINT('Ctrl Pts',(1.99169810931893,1.,0.157533331459215));
#32373=CARTESIAN_POINT('Ctrl Pts',(1.99753284771487,1.,0.155904629548774));
#32374=CARTESIAN_POINT('Ctrl Pts',(2.00335565310539,1.,0.154221403049719));
#32375=CARTESIAN_POINT('Ctrl Pts',(2.00917680318426,1.,0.152484883621452));
#32376=CARTESIAN_POINT('Ctrl Pts',(2.01500291940243,1.,0.150696157673084));
#32377=CARTESIAN_POINT('Ctrl Pts',(2.02083464969897,1.,0.148856124775342));
#32378=CARTESIAN_POINT('Ctrl Pts',(2.02666926182017,1.,0.146965557332586));
#32379=CARTESIAN_POINT('Ctrl Pts',(2.03250223739941,1.,0.145025140186058));
#32380=CARTESIAN_POINT('Ctrl Pts',(2.03832911025913,1.,0.143035515058208));
#32381=CARTESIAN_POINT('Ctrl Pts',(2.04414757947919,1.,0.140997332152545));
#32382=CARTESIAN_POINT('Ctrl Pts',(2.04995762001333,1.,0.138911255368966));
#32383=CARTESIAN_POINT('Ctrl Pts',(2.0557604441427,1.,0.136777941218044));
#32384=CARTESIAN_POINT('Ctrl Pts',(2.06155781517844,1.,0.134598026192107));
#32385=CARTESIAN_POINT('Ctrl Pts',(2.06735123910319,1.,0.132372111547709));
#32386=CARTESIAN_POINT('Ctrl Pts',(2.07314114713047,1.,0.1301007483284));
#32387=CARTESIAN_POINT('Ctrl Pts',(2.07892715110967,1.,0.127784445276116));
#32388=CARTESIAN_POINT('Ctrl Pts',(2.08470840653628,1.,0.125423679412058));
#32389=CARTESIAN_POINT('Ctrl Pts',(2.09048392424826,1.,0.123018905621083));
#32390=CARTESIAN_POINT('Ctrl Pts',(2.09625292867756,1.,0.120570567965129));
#32391=CARTESIAN_POINT('Ctrl Pts',(2.10201512132945,1.,0.118079107988368));
#32392=CARTESIAN_POINT('Ctrl Pts',(2.10777050261359,1.,0.11554495768794));
#32393=CARTESIAN_POINT('Ctrl Pts',(2.11351924490335,1.,0.112968534419746));
#32394=CARTESIAN_POINT('Ctrl Pts',(2.11926155590849,1.,0.11035023613502));
#32395=CARTESIAN_POINT('Ctrl Pts',(2.12499752306927,1.,0.107690435231068));
#32396=CARTESIAN_POINT('Ctrl Pts',(2.1307270488718,1.,0.104989479152703));
#32397=CARTESIAN_POINT('Ctrl Pts',(2.13644992667052,1.,0.102247700556063));
#32398=CARTESIAN_POINT('Ctrl Pts',(2.14216588395974,1.,0.0994654261990741));
#32399=CARTESIAN_POINT('Ctrl Pts',(2.14787463531864,1.,0.0966429852305688));
#32400=CARTESIAN_POINT('Ctrl Pts',(2.15357593978377,1.,0.0937807218868344));
#32401=CARTESIAN_POINT('Ctrl Pts',(2.15926961544808,1.,0.0908789888108265));
#32402=CARTESIAN_POINT('Ctrl Pts',(2.16495552645275,1.,0.0879381291387821));
#32403=CARTESIAN_POINT('Ctrl Pts',(2.17063357871031,1.,0.0849584620835642));
#32404=CARTESIAN_POINT('Ctrl Pts',(2.1763037121106,1.,0.0819402680871938));
#32405=CARTESIAN_POINT('Ctrl Pts',(2.18196589448304,1.,0.0788837727683226));
#32406=CARTESIAN_POINT('Ctrl Pts',(2.1876201139874,1.,0.075789146583341));
#32407=CARTESIAN_POINT('Ctrl Pts',(2.19213712012956,1.,0.0732830357304275));
#32408=CARTESIAN_POINT('Ctrl Pts',(2.19552129483562,1.,0.0713863779524626));
#32409=CARTESIAN_POINT('Ctrl Pts',(2.19777582085261,1.,0.0701143536324925));
#32410=CARTESIAN_POINT('Ctrl Pts',(2.19890268624765,1.,0.0694764450219582));
#32411=CARTESIAN_POINT('',(1.74236521665491,0.,0.163289472382896));
#32412=CARTESIAN_POINT('Origin',(0.,1.,0.));
#32413=CARTESIAN_POINT('Origin',(0.,1.,0.));
#32414=CARTESIAN_POINT('Origin',(0.,0.,0.));
#32415=CARTESIAN_POINT('',(0.,0.,0.));
#32416=CARTESIAN_POINT('Origin',(0.,0.,0.));
#32417=CARTESIAN_POINT('',(-0.32,0.16,3.91886975727153E-17));
#32418=CARTESIAN_POINT('Origin',(0.,0.16,0.));
#32419=CARTESIAN_POINT('',(-0.32,0.,3.91886975727153E-17));
#32420=CARTESIAN_POINT('',(-0.32,0.,3.91886975727153E-17));
#32421=CARTESIAN_POINT('Origin',(0.,0.,0.));
#32422=CARTESIAN_POINT('Origin',(0.,0.,0.));
#32423=CARTESIAN_POINT('',(-0.6,0.16,7.34788079488412E-17));
#32424=CARTESIAN_POINT('Origin',(0.,0.16,0.));
#32425=CARTESIAN_POINT('',(-0.6,0.,7.34788079488412E-17));
#32426=CARTESIAN_POINT('',(-0.6,0.,7.34788079488412E-17));
#32427=CARTESIAN_POINT('Origin',(0.,0.,0.));
#32428=CARTESIAN_POINT('Origin',(0.,0.16,0.));
#32429=CARTESIAN_POINT('Origin',(0.,0.,0.));
#32430=CARTESIAN_POINT('',(0.,0.,0.));
#32431=CARTESIAN_POINT('Origin',(0.45,0.6,0.));
#32432=CARTESIAN_POINT('',(-0.45,0.6,-5.51091059616309E-17));
#32433=CARTESIAN_POINT('Origin',(0.,0.6,0.));
#32434=CARTESIAN_POINT('Origin',(0.,0.575,0.));
#32435=CARTESIAN_POINT('',(-0.5,0.55,-6.12323399573677E-17));
#32436=CARTESIAN_POINT('Origin',(0.,0.55,0.));
#32437=CARTESIAN_POINT('',(-0.475,0.575,-5.81707229594993E-17));
#32438=CARTESIAN_POINT('Origin',(0.,0.29,0.));
#32439=CARTESIAN_POINT('',(-0.5,0.0299999999999998,-6.12323399573677E-17));
#32440=CARTESIAN_POINT('Origin',(0.,0.0299999999999998,0.));
#32441=CARTESIAN_POINT('',(-0.5,0.29,-6.12323399573677E-17));
#32442=CARTESIAN_POINT('Origin',(0.,0.0150000000000001,0.));
#32443=CARTESIAN_POINT('',(-0.47,7.11236625150491E-17,-5.75583995599256E-17));
#32444=CARTESIAN_POINT('Origin',(0.,0.,0.));
#32445=CARTESIAN_POINT('',(-0.485,0.0150000000000001,-5.93953697586466E-17));
#32446=CARTESIAN_POINT('Origin',(0.32,0.,0.));
#32447=CARTESIAN_POINT('',(-0.32,-6.93889390390723E-18,-3.91886975727153E-17));
#32448=CARTESIAN_POINT('Origin',(0.,0.,0.));
#32449=CARTESIAN_POINT('Origin',(0.,-0.02,0.));
#32450=CARTESIAN_POINT('',(-0.2942,-0.0515999999999999,3.60291088309151E-17));
#32451=CARTESIAN_POINT('Origin',(0.,-0.0515999999999999,0.));
#32452=CARTESIAN_POINT('',(-0.31,-0.02,-3.7964050773568E-17));
#32453=CARTESIAN_POINT('Origin',(0.,-1.24,0.));
#32454=CARTESIAN_POINT('',(-0.2942,-2.4458,3.60291088309151E-17));
#32455=CARTESIAN_POINT('Origin',(0.,-2.4458,0.));
#32456=CARTESIAN_POINT('',(-0.2942,-1.24,-3.60291088309151E-17));
#32457=CARTESIAN_POINT('Origin',(0.,-2.47,0.));
#32458=CARTESIAN_POINT('',(-0.24,-2.5,-2.93915231795365E-17));
#32459=CARTESIAN_POINT('Origin',(0.,-2.5,0.));
#32460=CARTESIAN_POINT('',(-0.27,-2.47,-3.30654635769785E-17));
#32461=CARTESIAN_POINT('Origin',(0.,-2.5,0.));
#32462=CARTESIAN_POINT('Origin',(0.144337567297406,-0.6,-0.25));
#32463=CARTESIAN_POINT('',(0.288675134594813,-0.6,0.));
#32464=CARTESIAN_POINT('',(0.144337567297406,-0.6,-0.25));
#32465=CARTESIAN_POINT('',(0.288675134594813,-0.6,0.));
#32466=CARTESIAN_POINT('',(0.144337567297406,-0.96,-0.25));
#32467=CARTESIAN_POINT('',(0.144337567297406,-0.6,-0.25));
#32468=CARTESIAN_POINT('',(0.288675134594813,-0.96,0.));
#32469=CARTESIAN_POINT('',(0.288675134594813,-0.96,0.));
#32470=CARTESIAN_POINT('',(0.288675134594813,-0.6,0.));
#32471=CARTESIAN_POINT('Origin',(-0.144337567297406,-0.6,-0.25));
#32472=CARTESIAN_POINT('',(-0.144337567297406,-0.6,-0.25));
#32473=CARTESIAN_POINT('',(0.144337567297406,-0.6,-0.25));
#32474=CARTESIAN_POINT('',(-0.144337567297406,-0.96,-0.25));
#32475=CARTESIAN_POINT('',(-0.144337567297406,-0.6,-0.25));
#32476=CARTESIAN_POINT('',(0.144337567297406,-0.96,-0.25));
#32477=CARTESIAN_POINT('Origin',(-0.288675134594813,-0.6,-8.32667268468867E-17));
#32478=CARTESIAN_POINT('',(-0.288675134594813,-0.6,-3.53525079574969E-17));
#32479=CARTESIAN_POINT('',(-0.144337567297406,-0.6,-0.25));
#32480=CARTESIAN_POINT('',(-0.288675134594813,-0.96,-5.55111512312578E-17));
#32481=CARTESIAN_POINT('',(-0.288675134594813,-0.6,-3.53525079574969E-17));
#32482=CARTESIAN_POINT('',(-0.144337567297406,-0.96,-0.25));
#32483=CARTESIAN_POINT('Origin',(-0.144337567297407,-0.6,0.25));
#32484=CARTESIAN_POINT('',(-0.144337567297407,-0.6,0.25));
#32485=CARTESIAN_POINT('',(-0.288675134594813,-0.6,-3.53525079574969E-17));
#32486=CARTESIAN_POINT('',(-0.144337567297407,-0.96,0.25));
#32487=CARTESIAN_POINT('',(-0.144337567297407,-0.6,0.25));
#32488=CARTESIAN_POINT('',(-0.288675134594813,-0.96,-3.53525079574969E-17));
#32489=CARTESIAN_POINT('Origin',(0.144337567297406,-0.6,0.25));
#32490=CARTESIAN_POINT('',(0.144337567297406,-0.6,0.25));
#32491=CARTESIAN_POINT('',(-0.144337567297407,-0.6,0.25));
#32492=CARTESIAN_POINT('',(0.144337567297406,-0.96,0.25));
#32493=CARTESIAN_POINT('',(0.144337567297406,-0.6,0.25));
#32494=CARTESIAN_POINT('',(-0.144337567297407,-0.96,0.25));
#32495=CARTESIAN_POINT('Origin',(0.288675134594813,-0.6,0.));
#32496=CARTESIAN_POINT('',(0.144337567297406,-0.6,0.25));
#32497=CARTESIAN_POINT('',(0.144337567297406,-0.96,0.25));
#32498=CARTESIAN_POINT('Origin',(0.,-0.6,0.));
#32499=CARTESIAN_POINT('Origin',(0.,-0.96,0.));
#32500=CARTESIAN_POINT('',(0.,0.,0.));
#32501=CARTESIAN_POINT('Origin',(0.3,0.4,0.));
#32502=CARTESIAN_POINT('',(-0.3,0.4,-3.67394039744206E-17));
#32503=CARTESIAN_POINT('Origin',(0.,0.4,0.));
#32504=CARTESIAN_POINT('Origin',(0.,0.375,0.));
#32505=CARTESIAN_POINT('',(-0.35,0.35,-4.28626379701573E-17));
#32506=CARTESIAN_POINT('Origin',(0.,0.35,0.));
#32507=CARTESIAN_POINT('',(-0.325,0.375,-3.9801020972289E-17));
#32508=CARTESIAN_POINT('Origin',(0.,0.19,0.));
#32509=CARTESIAN_POINT('',(-0.35,0.03,-4.28626379701574E-17));
#32510=CARTESIAN_POINT('Origin',(0.,0.03,0.));
#32511=CARTESIAN_POINT('',(-0.35,0.19,-4.28626379701574E-17));
#32512=CARTESIAN_POINT('Origin',(0.,0.0149999999999999,0.));
#32513=CARTESIAN_POINT('',(-0.32,-3.29597460435593E-17,-3.91886975727153E-17));
#32514=CARTESIAN_POINT('Origin',(0.,0.,0.));
#32515=CARTESIAN_POINT('',(-0.335,0.0149999999999999,-4.10256677714363E-17));
#32516=CARTESIAN_POINT('Origin',(0.22,0.,0.));
#32517=CARTESIAN_POINT('',(-0.22,-6.93889390390723E-18,-2.69422295812418E-17));
#32518=CARTESIAN_POINT('Origin',(0.,0.,0.));
#32519=CARTESIAN_POINT('Origin',(0.,-0.02,0.));
#32520=CARTESIAN_POINT('',(-0.1954,-0.0492,2.39295984553393E-17));
#32521=CARTESIAN_POINT('Origin',(0.,-0.0492,0.));
#32522=CARTESIAN_POINT('',(-0.21,-0.02,-2.57175827820944E-17));
#32523=CARTESIAN_POINT('Origin',(0.,-0.8,0.));
#32524=CARTESIAN_POINT('',(-0.1954,-1.5646,2.39295984553393E-17));
#32525=CARTESIAN_POINT('Origin',(0.,-1.5646,0.));
#32526=CARTESIAN_POINT('',(-0.1954,-0.8,-2.39295984553393E-17));
#32527=CARTESIAN_POINT('Origin',(0.,-1.58,0.));
#32528=CARTESIAN_POINT('',(-0.16,-1.6,-1.95943487863577E-17));
#32529=CARTESIAN_POINT('Origin',(0.,-1.6,0.));
#32530=CARTESIAN_POINT('',(-0.18,-1.58,-2.20436423846524E-17));
#32531=CARTESIAN_POINT('Origin',(0.,-1.6,0.));
#32532=CARTESIAN_POINT('Origin',(0.0866025403784439,-0.4,-0.15));
#32533=CARTESIAN_POINT('',(0.173205080756888,-0.4,0.));
#32534=CARTESIAN_POINT('',(0.0866025403784439,-0.4,-0.15));
#32535=CARTESIAN_POINT('',(0.173205080756888,-0.4,0.));
#32536=CARTESIAN_POINT('',(0.0866025403784439,-0.64,-0.15));
#32537=CARTESIAN_POINT('',(0.0866025403784439,-0.4,-0.15));
#32538=CARTESIAN_POINT('',(0.173205080756888,-0.64,0.));
#32539=CARTESIAN_POINT('',(0.173205080756888,-0.64,0.));
#32540=CARTESIAN_POINT('',(0.173205080756888,-0.4,0.));
#32541=CARTESIAN_POINT('Origin',(-0.0866025403784438,-0.4,-0.15));
#32542=CARTESIAN_POINT('',(-0.0866025403784438,-0.4,-0.15));
#32543=CARTESIAN_POINT('',(0.0866025403784439,-0.4,-0.15));
#32544=CARTESIAN_POINT('',(-0.0866025403784438,-0.64,-0.15));
#32545=CARTESIAN_POINT('',(-0.0866025403784438,-0.4,-0.15));
#32546=CARTESIAN_POINT('',(0.0866025403784439,-0.64,-0.15));
#32547=CARTESIAN_POINT('Origin',(-0.173205080756888,-0.4,-2.77555756156289E-17));
#32548=CARTESIAN_POINT('',(-0.173205080756888,-0.4,-2.12115047744981E-17));
#32549=CARTESIAN_POINT('',(-0.0866025403784438,-0.4,-0.15));
#32550=CARTESIAN_POINT('',(-0.173205080756888,-0.64,-2.77555756156289E-17));
#32551=CARTESIAN_POINT('',(-0.173205080756888,-0.4,-2.12115047744981E-17));
#32552=CARTESIAN_POINT('',(-0.0866025403784438,-0.64,-0.15));
#32553=CARTESIAN_POINT('Origin',(-0.0866025403784439,-0.4,0.15));
#32554=CARTESIAN_POINT('',(-0.0866025403784439,-0.4,0.15));
#32555=CARTESIAN_POINT('',(-0.173205080756888,-0.4,-2.12115047744981E-17));
#32556=CARTESIAN_POINT('',(-0.0866025403784439,-0.64,0.15));
#32557=CARTESIAN_POINT('',(-0.0866025403784439,-0.4,0.15));
#32558=CARTESIAN_POINT('',(-0.173205080756888,-0.64,-2.12115047744981E-17));
#32559=CARTESIAN_POINT('Origin',(0.0866025403784439,-0.4,0.15));
#32560=CARTESIAN_POINT('',(0.0866025403784439,-0.4,0.15));
#32561=CARTESIAN_POINT('',(-0.0866025403784439,-0.4,0.15));
#32562=CARTESIAN_POINT('',(0.0866025403784439,-0.64,0.15));
#32563=CARTESIAN_POINT('',(0.0866025403784439,-0.4,0.15));
#32564=CARTESIAN_POINT('',(-0.0866025403784439,-0.64,0.15));
#32565=CARTESIAN_POINT('Origin',(0.173205080756888,-0.4,0.));
#32566=CARTESIAN_POINT('',(0.0866025403784439,-0.4,0.15));
#32567=CARTESIAN_POINT('',(0.0866025403784439,-0.64,0.15));
#32568=CARTESIAN_POINT('Origin',(0.,-0.4,-2.77555756156289E-17));
#32569=CARTESIAN_POINT('Origin',(0.,-0.64,-2.77555756156289E-17));
#32570=CARTESIAN_POINT('',(0.,0.,0.));
#32571=CARTESIAN_POINT('',(0.,0.,0.));
#32572=CARTESIAN_POINT('',(0.,0.,0.));
#32573=CARTESIAN_POINT('',(0.,0.,0.));
#32574=CARTESIAN_POINT('',(0.,0.,0.));
#32575=CARTESIAN_POINT('',(0.,0.,0.));
#32576=CARTESIAN_POINT('',(0.,0.,0.));
#32577=CARTESIAN_POINT('',(0.,0.,0.));
#32578=CARTESIAN_POINT('',(0.,0.,0.));
#32579=CARTESIAN_POINT('',(0.,0.,0.));
#32580=CARTESIAN_POINT('',(0.,0.,0.));
#32581=CARTESIAN_POINT('',(0.,0.,0.));
#32582=CARTESIAN_POINT('',(0.,0.,0.));
#32583=CARTESIAN_POINT('',(0.,0.,0.));
#32584=CARTESIAN_POINT('',(0.,0.,0.));
#32585=CARTESIAN_POINT('',(4.,-3.2,2.));
#32586=CARTESIAN_POINT('',(4.,3.2,2.));
#32587=CARTESIAN_POINT('',(7.,-3.2,2.));
#32588=CARTESIAN_POINT('',(7.,3.2,2.));
#32589=CARTESIAN_POINT('',(2.4,-1.6,15.6));
#32590=CARTESIAN_POINT('',(2.4,1.6,15.6));
#32591=CARTESIAN_POINT('',(2.4,-1.6,25.6));
#32592=CARTESIAN_POINT('',(2.4,1.6,25.6));
#32593=CARTESIAN_POINT('',(1.,-1.8,1.6));
#32594=CARTESIAN_POINT('',(1.,1.8,1.6));
#32595=CARTESIAN_POINT('',(-6.05,-3.,1.8));
#32596=CARTESIAN_POINT('',(-0.45,-3.,1.8));
#32597=CARTESIAN_POINT('',(-3.25,-3.,20.));
#32598=CARTESIAN_POINT('',(-1.8357864376269,-4.,21.4142135623731));
#32599=CARTESIAN_POINT('',(-4.66421356237309,-4.,21.4142135623731));
#32600=CARTESIAN_POINT('',(-4.66421356237309,-4.,18.5857864376269));
#32601=CARTESIAN_POINT('',(-1.83578643762691,-4.,18.5857864376269));
#32602=CARTESIAN_POINT('',(-1.8357864376269,-2.,21.4142135623731));
#32603=CARTESIAN_POINT('',(-4.66421356237309,-2.,21.4142135623731));
#32604=CARTESIAN_POINT('',(-4.66421356237309,-2.,18.5857864376269));
#32605=CARTESIAN_POINT('',(-1.83578643762691,-2.,18.5857864376269));
#32606=CARTESIAN_POINT('',(-6.05,3.,1.8));
#32607=CARTESIAN_POINT('',(-0.45,3.,1.8));
#32608=CARTESIAN_POINT('',(-3.25,3.,20.));
#32609=CARTESIAN_POINT('',(-1.8357864376269,2.,21.4142135623731));
#32610=CARTESIAN_POINT('',(-4.66421356237309,2.,21.4142135623731));
#32611=CARTESIAN_POINT('',(-4.66421356237309,2.,18.5857864376269));
#32612=CARTESIAN_POINT('',(-1.83578643762691,2.,18.5857864376269));
#32613=CARTESIAN_POINT('',(-1.8357864376269,4.,21.4142135623731));
#32614=CARTESIAN_POINT('',(-4.66421356237309,4.,21.4142135623731));
#32615=CARTESIAN_POINT('',(-4.66421356237309,4.,18.5857864376269));
#32616=CARTESIAN_POINT('',(-1.83578643762691,4.,18.5857864376269));
#32617=CARTESIAN_POINT('',(0.,0.,0.));
#32618=CARTESIAN_POINT('',(0.,0.,0.));
#32619=CARTESIAN_POINT('',(0.,0.,0.));
#32620=CARTESIAN_POINT('',(0.,0.,0.));
#32621=CARTESIAN_POINT('',(0.,0.,0.));
#32622=CARTESIAN_POINT('',(0.,0.,0.));
#32623=CARTESIAN_POINT('',(0.,0.,0.));
#32624=CARTESIAN_POINT('',(0.,0.,0.));
#32625=CARTESIAN_POINT('',(0.,0.,0.));
#32626=CARTESIAN_POINT('',(0.,0.,0.));
#32627=CARTESIAN_POINT('',(0.,0.,0.));
#32628=CARTESIAN_POINT('',(-3.25,0.,20.));
#32629=CARTESIAN_POINT('',(-3.25,8.4,29.));
#32630=CARTESIAN_POINT('',(-3.25,8.56,29.));
#32631=CARTESIAN_POINT('',(-3.25,-5.7,20.));
#32632=CARTESIAN_POINT('',(-3.25,7.7,20.));
#32633=CARTESIAN_POINT('',(0.,0.,0.));
#32634=CARTESIAN_POINT('',(0.,0.,0.));
#32635=CARTESIAN_POINT('Origin',(-3.25,6.8,29.));
#32636=CARTESIAN_POINT('',(-3.655,8.37,29.));
#32637=CARTESIAN_POINT('Origin',(-3.25,8.37,29.));
#32638=CARTESIAN_POINT('',(-3.655,6.8,29.));
#32639=CARTESIAN_POINT('',(-3.655,6.8,29.));
#32640=CARTESIAN_POINT('Origin',(-3.25,6.8,29.));
#32641=CARTESIAN_POINT('Origin',(-3.25,6.8,29.));
#32642=CARTESIAN_POINT('',(-4.15,8.37,29.));
#32643=CARTESIAN_POINT('Origin',(-3.25,8.37,29.));
#32644=CARTESIAN_POINT('',(-4.15,6.8,29.));
#32645=CARTESIAN_POINT('',(-4.15,6.8,29.));
#32646=CARTESIAN_POINT('Origin',(-3.25,6.8,29.));
#32647=CARTESIAN_POINT('Origin',(-3.25,8.37,29.));
#32648=CARTESIAN_POINT('Origin',(-3.25,6.8,29.));
#32649=CARTESIAN_POINT('',(0.,0.,0.));
#32650=CARTESIAN_POINT('',(0.,0.,0.));
#32651=CARTESIAN_POINT('',(0.,0.,0.));
#32652=CARTESIAN_POINT('',(0.,0.,0.));
#32653=CARTESIAN_POINT('',(0.,0.,0.));
#32654=UNCERTAINTY_MEASURE_WITH_UNIT(LENGTH_MEASURE(0.001),#32752,
'DISTANCE_ACCURACY_VALUE',
'Maximum model space distance between geometric entities at asserted c
onnectivities');
#32655=UNCERTAINTY_MEASURE_WITH_UNIT(LENGTH_MEASURE(0.001),#32752,
'DISTANCE_ACCURACY_VALUE',
'Maximum model space distance between geometric entities at asserted c
onnectivities');
#32656=UNCERTAINTY_MEASURE_WITH_UNIT(LENGTH_MEASURE(0.001),#32752,
'DISTANCE_ACCURACY_VALUE',
'Maximum model space distance between geometric entities at asserted c
onnectivities');
#32657=UNCERTAINTY_MEASURE_WITH_UNIT(LENGTH_MEASURE(0.001),#32752,
'DISTANCE_ACCURACY_VALUE',
'Maximum model space distance between geometric entities at asserted c
onnectivities');
#32658=UNCERTAINTY_MEASURE_WITH_UNIT(LENGTH_MEASURE(0.001),#32752,
'DISTANCE_ACCURACY_VALUE',
'Maximum model space distance between geometric entities at asserted c
onnectivities');
#32659=UNCERTAINTY_MEASURE_WITH_UNIT(LENGTH_MEASURE(0.001),#32752,
'DISTANCE_ACCURACY_VALUE',
'Maximum model space distance between geometric entities at asserted c
onnectivities');
#32660=UNCERTAINTY_MEASURE_WITH_UNIT(LENGTH_MEASURE(0.001),#32752,
'DISTANCE_ACCURACY_VALUE',
'Maximum model space distance between geometric entities at asserted c
onnectivities');
#32661=UNCERTAINTY_MEASURE_WITH_UNIT(LENGTH_MEASURE(0.001),#32752,
'DISTANCE_ACCURACY_VALUE',
'Maximum model space distance between geometric entities at asserted c
onnectivities');
#32662=UNCERTAINTY_MEASURE_WITH_UNIT(LENGTH_MEASURE(0.001),#32752,
'DISTANCE_ACCURACY_VALUE',
'Maximum model space distance between geometric entities at asserted c
onnectivities');
#32663=UNCERTAINTY_MEASURE_WITH_UNIT(LENGTH_MEASURE(0.001),#32752,
'DISTANCE_ACCURACY_VALUE',
'Maximum model space distance between geometric entities at asserted c
onnectivities');
#32664=UNCERTAINTY_MEASURE_WITH_UNIT(LENGTH_MEASURE(0.001),#32752,
'DISTANCE_ACCURACY_VALUE',
'Maximum model space distance between geometric entities at asserted c
onnectivities');
#32665=UNCERTAINTY_MEASURE_WITH_UNIT(LENGTH_MEASURE(0.001),#32752,
'DISTANCE_ACCURACY_VALUE',
'Maximum model space distance between geometric entities at asserted c
onnectivities');
#32666=UNCERTAINTY_MEASURE_WITH_UNIT(LENGTH_MEASURE(0.001),#32752,
'DISTANCE_ACCURACY_VALUE',
'Maximum model space distance between geometric entities at asserted c
onnectivities');
#32667=UNCERTAINTY_MEASURE_WITH_UNIT(LENGTH_MEASURE(0.001),#32752,
'DISTANCE_ACCURACY_VALUE',
'Maximum model space distance between geometric entities at asserted c
onnectivities');
#32668=UNCERTAINTY_MEASURE_WITH_UNIT(LENGTH_MEASURE(0.001),#32752,
'DISTANCE_ACCURACY_VALUE',
'Maximum model space distance between geometric entities at asserted c
onnectivities');
#32669=UNCERTAINTY_MEASURE_WITH_UNIT(LENGTH_MEASURE(0.001),#32752,
'DISTANCE_ACCURACY_VALUE',
'Maximum model space distance between geometric entities at asserted c
onnectivities');
#32670=UNCERTAINTY_MEASURE_WITH_UNIT(LENGTH_MEASURE(0.001),#32752,
'DISTANCE_ACCURACY_VALUE',
'Maximum model space distance between geometric entities at asserted c
onnectivities');
#32671=UNCERTAINTY_MEASURE_WITH_UNIT(LENGTH_MEASURE(0.001),#32752,
'DISTANCE_ACCURACY_VALUE',
'Maximum model space distance between geometric entities at asserted c
onnectivities');
#32672=UNCERTAINTY_MEASURE_WITH_UNIT(LENGTH_MEASURE(0.001),#32752,
'DISTANCE_ACCURACY_VALUE',
'Maximum model space distance between geometric entities at asserted c
onnectivities');
#32673=UNCERTAINTY_MEASURE_WITH_UNIT(LENGTH_MEASURE(0.001),#32752,
'DISTANCE_ACCURACY_VALUE',
'Maximum model space distance between geometric entities at asserted c
onnectivities');
#32674=UNCERTAINTY_MEASURE_WITH_UNIT(LENGTH_MEASURE(0.001),#32752,
'DISTANCE_ACCURACY_VALUE',
'Maximum model space distance between geometric entities at asserted c
onnectivities');
#32675=UNCERTAINTY_MEASURE_WITH_UNIT(LENGTH_MEASURE(0.001),#32752,
'DISTANCE_ACCURACY_VALUE',
'Maximum model space distance between geometric entities at asserted c
onnectivities');
#32676=UNCERTAINTY_MEASURE_WITH_UNIT(LENGTH_MEASURE(0.001),#32752,
'DISTANCE_ACCURACY_VALUE',
'Maximum model space distance between geometric entities at asserted c
onnectivities');
#32677=UNCERTAINTY_MEASURE_WITH_UNIT(LENGTH_MEASURE(0.001),#32752,
'DISTANCE_ACCURACY_VALUE',
'Maximum model space distance between geometric entities at asserted c
onnectivities');
#32678=UNCERTAINTY_MEASURE_WITH_UNIT(LENGTH_MEASURE(0.001),#32752,
'DISTANCE_ACCURACY_VALUE',
'Maximum model space distance between geometric entities at asserted c
onnectivities');
#32679=UNCERTAINTY_MEASURE_WITH_UNIT(LENGTH_MEASURE(0.001),#32752,
'DISTANCE_ACCURACY_VALUE',
'Maximum model space distance between geometric entities at asserted c
onnectivities');
#32680=UNCERTAINTY_MEASURE_WITH_UNIT(LENGTH_MEASURE(0.001),#32752,
'DISTANCE_ACCURACY_VALUE',
'Maximum model space distance between geometric entities at asserted c
onnectivities');
#32681=UNCERTAINTY_MEASURE_WITH_UNIT(LENGTH_MEASURE(0.001),#32752,
'DISTANCE_ACCURACY_VALUE',
'Maximum model space distance between geometric entities at asserted c
onnectivities');
#32682=UNCERTAINTY_MEASURE_WITH_UNIT(LENGTH_MEASURE(0.001),#32752,
'DISTANCE_ACCURACY_VALUE',
'Maximum model space distance between geometric entities at asserted c
onnectivities');
#32683=UNCERTAINTY_MEASURE_WITH_UNIT(LENGTH_MEASURE(0.001),#32752,
'DISTANCE_ACCURACY_VALUE',
'Maximum model space distance between geometric entities at asserted c
onnectivities');
#32684=UNCERTAINTY_MEASURE_WITH_UNIT(LENGTH_MEASURE(0.001),#32752,
'DISTANCE_ACCURACY_VALUE',
'Maximum model space distance between geometric entities at asserted c
onnectivities');
#32685=UNCERTAINTY_MEASURE_WITH_UNIT(LENGTH_MEASURE(0.001),#32752,
'DISTANCE_ACCURACY_VALUE',
'Maximum model space distance between geometric entities at asserted c
onnectivities');
#32686=UNCERTAINTY_MEASURE_WITH_UNIT(LENGTH_MEASURE(0.001),#32752,
'DISTANCE_ACCURACY_VALUE',
'Maximum model space distance between geometric entities at asserted c
onnectivities');
#32687=UNCERTAINTY_MEASURE_WITH_UNIT(LENGTH_MEASURE(0.001),#32752,
'DISTANCE_ACCURACY_VALUE',
'Maximum model space distance between geometric entities at asserted c
onnectivities');
#32688=UNCERTAINTY_MEASURE_WITH_UNIT(LENGTH_MEASURE(0.001),#32752,
'DISTANCE_ACCURACY_VALUE',
'Maximum model space distance between geometric entities at asserted c
onnectivities');
#32689=UNCERTAINTY_MEASURE_WITH_UNIT(LENGTH_MEASURE(0.001),#32752,
'DISTANCE_ACCURACY_VALUE',
'Maximum model space distance between geometric entities at asserted c
onnectivities');
#32690=UNCERTAINTY_MEASURE_WITH_UNIT(LENGTH_MEASURE(0.001),#32752,
'DISTANCE_ACCURACY_VALUE',
'Maximum model space distance between geometric entities at asserted c
onnectivities');
#32691=UNCERTAINTY_MEASURE_WITH_UNIT(LENGTH_MEASURE(0.001),#32752,
'DISTANCE_ACCURACY_VALUE',
'Maximum model space distance between geometric entities at asserted c
onnectivities');
#32692=UNCERTAINTY_MEASURE_WITH_UNIT(LENGTH_MEASURE(0.001),#32752,
'DISTANCE_ACCURACY_VALUE',
'Maximum model space distance between geometric entities at asserted c
onnectivities');
#32693=UNCERTAINTY_MEASURE_WITH_UNIT(LENGTH_MEASURE(0.001),#32752,
'DISTANCE_ACCURACY_VALUE',
'Maximum model space distance between geometric entities at asserted c
onnectivities');
#32694=UNCERTAINTY_MEASURE_WITH_UNIT(LENGTH_MEASURE(0.001),#32752,
'DISTANCE_ACCURACY_VALUE',
'Maximum model space distance between geometric entities at asserted c
onnectivities');
#32695=UNCERTAINTY_MEASURE_WITH_UNIT(LENGTH_MEASURE(0.001),#32752,
'DISTANCE_ACCURACY_VALUE',
'Maximum model space distance between geometric entities at asserted c
onnectivities');
#32696=UNCERTAINTY_MEASURE_WITH_UNIT(LENGTH_MEASURE(0.001),#32752,
'DISTANCE_ACCURACY_VALUE',
'Maximum model space distance between geometric entities at asserted c
onnectivities');
#32697=UNCERTAINTY_MEASURE_WITH_UNIT(LENGTH_MEASURE(0.001),#32752,
'DISTANCE_ACCURACY_VALUE',
'Maximum model space distance between geometric entities at asserted c
onnectivities');
#32698=UNCERTAINTY_MEASURE_WITH_UNIT(LENGTH_MEASURE(0.001),#32752,
'DISTANCE_ACCURACY_VALUE',
'Maximum model space distance between geometric entities at asserted c
onnectivities');
#32699=UNCERTAINTY_MEASURE_WITH_UNIT(LENGTH_MEASURE(0.001),#32752,
'DISTANCE_ACCURACY_VALUE',
'Maximum model space distance between geometric entities at asserted c
onnectivities');
#32700=UNCERTAINTY_MEASURE_WITH_UNIT(LENGTH_MEASURE(0.001),#32752,
'DISTANCE_ACCURACY_VALUE',
'Maximum model space distance between geometric entities at asserted c
onnectivities');
#32701=UNCERTAINTY_MEASURE_WITH_UNIT(LENGTH_MEASURE(0.001),#32752,
'DISTANCE_ACCURACY_VALUE',
'Maximum model space distance between geometric entities at asserted c
onnectivities');
#32702=UNCERTAINTY_MEASURE_WITH_UNIT(LENGTH_MEASURE(0.001),#32752,
'DISTANCE_ACCURACY_VALUE',
'Maximum model space distance between geometric entities at asserted c
onnectivities');
#32703=(
GEOMETRIC_REPRESENTATION_CONTEXT(3)
GLOBAL_UNCERTAINTY_ASSIGNED_CONTEXT((#32654))
GLOBAL_UNIT_ASSIGNED_CONTEXT((#32752,#32754,#32755))
REPRESENTATION_CONTEXT('','3D')
);
#32704=(
GEOMETRIC_REPRESENTATION_CONTEXT(3)
GLOBAL_UNCERTAINTY_ASSIGNED_CONTEXT((#32655))
GLOBAL_UNIT_ASSIGNED_CONTEXT((#32752,#32754,#32755))
REPRESENTATION_CONTEXT('','3D')
);
#32705=(
GEOMETRIC_REPRESENTATION_CONTEXT(3)
GLOBAL_UNCERTAINTY_ASSIGNED_CONTEXT((#32656))
GLOBAL_UNIT_ASSIGNED_CONTEXT((#32752,#32754,#32755))
REPRESENTATION_CONTEXT('','3D')
);
#32706=(
GEOMETRIC_REPRESENTATION_CONTEXT(3)
GLOBAL_UNCERTAINTY_ASSIGNED_CONTEXT((#32657))
GLOBAL_UNIT_ASSIGNED_CONTEXT((#32752,#32754,#32755))
REPRESENTATION_CONTEXT('','3D')
);
#32707=(
GEOMETRIC_REPRESENTATION_CONTEXT(3)
GLOBAL_UNCERTAINTY_ASSIGNED_CONTEXT((#32658))
GLOBAL_UNIT_ASSIGNED_CONTEXT((#32752,#32754,#32755))
REPRESENTATION_CONTEXT('','3D')
);
#32708=(
GEOMETRIC_REPRESENTATION_CONTEXT(3)
GLOBAL_UNCERTAINTY_ASSIGNED_CONTEXT((#32659))
GLOBAL_UNIT_ASSIGNED_CONTEXT((#32752,#32754,#32755))
REPRESENTATION_CONTEXT('','3D')
);
#32709=(
GEOMETRIC_REPRESENTATION_CONTEXT(3)
GLOBAL_UNCERTAINTY_ASSIGNED_CONTEXT((#32660))
GLOBAL_UNIT_ASSIGNED_CONTEXT((#32752,#32754,#32755))
REPRESENTATION_CONTEXT('','3D')
);
#32710=(
GEOMETRIC_REPRESENTATION_CONTEXT(3)
GLOBAL_UNCERTAINTY_ASSIGNED_CONTEXT((#32661))
GLOBAL_UNIT_ASSIGNED_CONTEXT((#32752,#32754,#32755))
REPRESENTATION_CONTEXT('','3D')
);
#32711=(
GEOMETRIC_REPRESENTATION_CONTEXT(3)
GLOBAL_UNCERTAINTY_ASSIGNED_CONTEXT((#32662))
GLOBAL_UNIT_ASSIGNED_CONTEXT((#32752,#32754,#32755))
REPRESENTATION_CONTEXT('','3D')
);
#32712=(
GEOMETRIC_REPRESENTATION_CONTEXT(3)
GLOBAL_UNCERTAINTY_ASSIGNED_CONTEXT((#32663))
GLOBAL_UNIT_ASSIGNED_CONTEXT((#32752,#32754,#32755))
REPRESENTATION_CONTEXT('','3D')
);
#32713=(
GEOMETRIC_REPRESENTATION_CONTEXT(3)
GLOBAL_UNCERTAINTY_ASSIGNED_CONTEXT((#32664))
GLOBAL_UNIT_ASSIGNED_CONTEXT((#32752,#32754,#32755))
REPRESENTATION_CONTEXT('','3D')
);
#32714=(
GEOMETRIC_REPRESENTATION_CONTEXT(3)
GLOBAL_UNCERTAINTY_ASSIGNED_CONTEXT((#32665))
GLOBAL_UNIT_ASSIGNED_CONTEXT((#32752,#32754,#32755))
REPRESENTATION_CONTEXT('','3D')
);
#32715=(
GEOMETRIC_REPRESENTATION_CONTEXT(3)
GLOBAL_UNCERTAINTY_ASSIGNED_CONTEXT((#32666))
GLOBAL_UNIT_ASSIGNED_CONTEXT((#32752,#32754,#32755))
REPRESENTATION_CONTEXT('','3D')
);
#32716=(
GEOMETRIC_REPRESENTATION_CONTEXT(3)
GLOBAL_UNCERTAINTY_ASSIGNED_CONTEXT((#32667))
GLOBAL_UNIT_ASSIGNED_CONTEXT((#32752,#32754,#32755))
REPRESENTATION_CONTEXT('','3D')
);
#32717=(
GEOMETRIC_REPRESENTATION_CONTEXT(3)
GLOBAL_UNCERTAINTY_ASSIGNED_CONTEXT((#32668))
GLOBAL_UNIT_ASSIGNED_CONTEXT((#32752,#32754,#32755))
REPRESENTATION_CONTEXT('','3D')
);
#32718=(
GEOMETRIC_REPRESENTATION_CONTEXT(3)
GLOBAL_UNCERTAINTY_ASSIGNED_CONTEXT((#32669))
GLOBAL_UNIT_ASSIGNED_CONTEXT((#32752,#32754,#32755))
REPRESENTATION_CONTEXT('','3D')
);
#32719=(
GEOMETRIC_REPRESENTATION_CONTEXT(3)
GLOBAL_UNCERTAINTY_ASSIGNED_CONTEXT((#32670))
GLOBAL_UNIT_ASSIGNED_CONTEXT((#32752,#32754,#32755))
REPRESENTATION_CONTEXT('','3D')
);
#32720=(
GEOMETRIC_REPRESENTATION_CONTEXT(3)
GLOBAL_UNCERTAINTY_ASSIGNED_CONTEXT((#32671))
GLOBAL_UNIT_ASSIGNED_CONTEXT((#32752,#32754,#32755))
REPRESENTATION_CONTEXT('','3D')
);
#32721=(
GEOMETRIC_REPRESENTATION_CONTEXT(3)
GLOBAL_UNCERTAINTY_ASSIGNED_CONTEXT((#32672))
GLOBAL_UNIT_ASSIGNED_CONTEXT((#32752,#32754,#32755))
REPRESENTATION_CONTEXT('','3D')
);
#32722=(
GEOMETRIC_REPRESENTATION_CONTEXT(3)
GLOBAL_UNCERTAINTY_ASSIGNED_CONTEXT((#32673))
GLOBAL_UNIT_ASSIGNED_CONTEXT((#32752,#32754,#32755))
REPRESENTATION_CONTEXT('','3D')
);
#32723=(
GEOMETRIC_REPRESENTATION_CONTEXT(3)
GLOBAL_UNCERTAINTY_ASSIGNED_CONTEXT((#32674))
GLOBAL_UNIT_ASSIGNED_CONTEXT((#32752,#32754,#32755))
REPRESENTATION_CONTEXT('','3D')
);
#32724=(
GEOMETRIC_REPRESENTATION_CONTEXT(3)
GLOBAL_UNCERTAINTY_ASSIGNED_CONTEXT((#32675))
GLOBAL_UNIT_ASSIGNED_CONTEXT((#32752,#32754,#32755))
REPRESENTATION_CONTEXT('','3D')
);
#32725=(
GEOMETRIC_REPRESENTATION_CONTEXT(3)
GLOBAL_UNCERTAINTY_ASSIGNED_CONTEXT((#32676))
GLOBAL_UNIT_ASSIGNED_CONTEXT((#32752,#32754,#32755))
REPRESENTATION_CONTEXT('','3D')
);
#32726=(
GEOMETRIC_REPRESENTATION_CONTEXT(3)
GLOBAL_UNCERTAINTY_ASSIGNED_CONTEXT((#32677))
GLOBAL_UNIT_ASSIGNED_CONTEXT((#32752,#32754,#32755))
REPRESENTATION_CONTEXT('','3D')
);
#32727=(
GEOMETRIC_REPRESENTATION_CONTEXT(3)
GLOBAL_UNCERTAINTY_ASSIGNED_CONTEXT((#32678))
GLOBAL_UNIT_ASSIGNED_CONTEXT((#32752,#32754,#32755))
REPRESENTATION_CONTEXT('','3D')
);
#32728=(
GEOMETRIC_REPRESENTATION_CONTEXT(3)
GLOBAL_UNCERTAINTY_ASSIGNED_CONTEXT((#32679))
GLOBAL_UNIT_ASSIGNED_CONTEXT((#32752,#32754,#32755))
REPRESENTATION_CONTEXT('','3D')
);
#32729=(
GEOMETRIC_REPRESENTATION_CONTEXT(3)
GLOBAL_UNCERTAINTY_ASSIGNED_CONTEXT((#32680))
GLOBAL_UNIT_ASSIGNED_CONTEXT((#32752,#32754,#32755))
REPRESENTATION_CONTEXT('','3D')
);
#32730=(
GEOMETRIC_REPRESENTATION_CONTEXT(3)
GLOBAL_UNCERTAINTY_ASSIGNED_CONTEXT((#32681))
GLOBAL_UNIT_ASSIGNED_CONTEXT((#32752,#32754,#32755))
REPRESENTATION_CONTEXT('','3D')
);
#32731=(
GEOMETRIC_REPRESENTATION_CONTEXT(3)
GLOBAL_UNCERTAINTY_ASSIGNED_CONTEXT((#32682))
GLOBAL_UNIT_ASSIGNED_CONTEXT((#32752,#32754,#32755))
REPRESENTATION_CONTEXT('','3D')
);
#32732=(
GEOMETRIC_REPRESENTATION_CONTEXT(3)
GLOBAL_UNCERTAINTY_ASSIGNED_CONTEXT((#32683))
GLOBAL_UNIT_ASSIGNED_CONTEXT((#32752,#32754,#32755))
REPRESENTATION_CONTEXT('','3D')
);
#32733=(
GEOMETRIC_REPRESENTATION_CONTEXT(3)
GLOBAL_UNCERTAINTY_ASSIGNED_CONTEXT((#32684))
GLOBAL_UNIT_ASSIGNED_CONTEXT((#32752,#32754,#32755))
REPRESENTATION_CONTEXT('','3D')
);
#32734=(
GEOMETRIC_REPRESENTATION_CONTEXT(3)
GLOBAL_UNCERTAINTY_ASSIGNED_CONTEXT((#32685))
GLOBAL_UNIT_ASSIGNED_CONTEXT((#32752,#32754,#32755))
REPRESENTATION_CONTEXT('','3D')
);
#32735=(
GEOMETRIC_REPRESENTATION_CONTEXT(3)
GLOBAL_UNCERTAINTY_ASSIGNED_CONTEXT((#32686))
GLOBAL_UNIT_ASSIGNED_CONTEXT((#32752,#32754,#32755))
REPRESENTATION_CONTEXT('','3D')
);
#32736=(
GEOMETRIC_REPRESENTATION_CONTEXT(3)
GLOBAL_UNCERTAINTY_ASSIGNED_CONTEXT((#32687))
GLOBAL_UNIT_ASSIGNED_CONTEXT((#32752,#32754,#32755))
REPRESENTATION_CONTEXT('','3D')
);
#32737=(
GEOMETRIC_REPRESENTATION_CONTEXT(3)
GLOBAL_UNCERTAINTY_ASSIGNED_CONTEXT((#32688))
GLOBAL_UNIT_ASSIGNED_CONTEXT((#32752,#32754,#32755))
REPRESENTATION_CONTEXT('','3D')
);
#32738=(
GEOMETRIC_REPRESENTATION_CONTEXT(3)
GLOBAL_UNCERTAINTY_ASSIGNED_CONTEXT((#32689))
GLOBAL_UNIT_ASSIGNED_CONTEXT((#32752,#32754,#32755))
REPRESENTATION_CONTEXT('','3D')
);
#32739=(
GEOMETRIC_REPRESENTATION_CONTEXT(3)
GLOBAL_UNCERTAINTY_ASSIGNED_CONTEXT((#32690))
GLOBAL_UNIT_ASSIGNED_CONTEXT((#32752,#32754,#32755))
REPRESENTATION_CONTEXT('','3D')
);
#32740=(
GEOMETRIC_REPRESENTATION_CONTEXT(3)
GLOBAL_UNCERTAINTY_ASSIGNED_CONTEXT((#32691))
GLOBAL_UNIT_ASSIGNED_CONTEXT((#32752,#32754,#32755))
REPRESENTATION_CONTEXT('','3D')
);
#32741=(
GEOMETRIC_REPRESENTATION_CONTEXT(3)
GLOBAL_UNCERTAINTY_ASSIGNED_CONTEXT((#32692))
GLOBAL_UNIT_ASSIGNED_CONTEXT((#32752,#32754,#32755))
REPRESENTATION_CONTEXT('','3D')
);
#32742=(
GEOMETRIC_REPRESENTATION_CONTEXT(3)
GLOBAL_UNCERTAINTY_ASSIGNED_CONTEXT((#32693))
GLOBAL_UNIT_ASSIGNED_CONTEXT((#32752,#32754,#32755))
REPRESENTATION_CONTEXT('','3D')
);
#32743=(
GEOMETRIC_REPRESENTATION_CONTEXT(3)
GLOBAL_UNCERTAINTY_ASSIGNED_CONTEXT((#32694))
GLOBAL_UNIT_ASSIGNED_CONTEXT((#32752,#32754,#32755))
REPRESENTATION_CONTEXT('','3D')
);
#32744=(
GEOMETRIC_REPRESENTATION_CONTEXT(3)
GLOBAL_UNCERTAINTY_ASSIGNED_CONTEXT((#32695))
GLOBAL_UNIT_ASSIGNED_CONTEXT((#32752,#32754,#32755))
REPRESENTATION_CONTEXT('','3D')
);
#32745=(
GEOMETRIC_REPRESENTATION_CONTEXT(3)
GLOBAL_UNCERTAINTY_ASSIGNED_CONTEXT((#32696))
GLOBAL_UNIT_ASSIGNED_CONTEXT((#32752,#32754,#32755))
REPRESENTATION_CONTEXT('','3D')
);
#32746=(
GEOMETRIC_REPRESENTATION_CONTEXT(3)
GLOBAL_UNCERTAINTY_ASSIGNED_CONTEXT((#32697))
GLOBAL_UNIT_ASSIGNED_CONTEXT((#32752,#32754,#32755))
REPRESENTATION_CONTEXT('','3D')
);
#32747=(
GEOMETRIC_REPRESENTATION_CONTEXT(3)
GLOBAL_UNCERTAINTY_ASSIGNED_CONTEXT((#32698))
GLOBAL_UNIT_ASSIGNED_CONTEXT((#32752,#32754,#32755))
REPRESENTATION_CONTEXT('','3D')
);
#32748=(
GEOMETRIC_REPRESENTATION_CONTEXT(3)
GLOBAL_UNCERTAINTY_ASSIGNED_CONTEXT((#32699))
GLOBAL_UNIT_ASSIGNED_CONTEXT((#32752,#32754,#32755))
REPRESENTATION_CONTEXT('','3D')
);
#32749=(
GEOMETRIC_REPRESENTATION_CONTEXT(3)
GLOBAL_UNCERTAINTY_ASSIGNED_CONTEXT((#32700))
GLOBAL_UNIT_ASSIGNED_CONTEXT((#32752,#32754,#32755))
REPRESENTATION_CONTEXT('','3D')
);
#32750=(
GEOMETRIC_REPRESENTATION_CONTEXT(3)
GLOBAL_UNCERTAINTY_ASSIGNED_CONTEXT((#32701))
GLOBAL_UNIT_ASSIGNED_CONTEXT((#32752,#32754,#32755))
REPRESENTATION_CONTEXT('','3D')
);
#32751=(
GEOMETRIC_REPRESENTATION_CONTEXT(3)
GLOBAL_UNCERTAINTY_ASSIGNED_CONTEXT((#32702))
GLOBAL_UNIT_ASSIGNED_CONTEXT((#32752,#32754,#32755))
REPRESENTATION_CONTEXT('','3D')
);
#32752=(
LENGTH_UNIT()
NAMED_UNIT(*)
SI_UNIT(.CENTI.,.METRE.)
);
#32753=(
LENGTH_UNIT()
NAMED_UNIT(*)
SI_UNIT($,.METRE.)
);
#32754=(
NAMED_UNIT(*)
PLANE_ANGLE_UNIT()
SI_UNIT($,.RADIAN.)
);
#32755=(
NAMED_UNIT(*)
SI_UNIT($,.STERADIAN.)
SOLID_ANGLE_UNIT()
);
#32756=SHAPE_DEFINITION_REPRESENTATION(#32804,#32929);
#32757=SHAPE_DEFINITION_REPRESENTATION(#32805,#32930);
#32758=SHAPE_DEFINITION_REPRESENTATION(#32806,#32931);
#32759=SHAPE_DEFINITION_REPRESENTATION(#32807,#32932);
#32760=SHAPE_DEFINITION_REPRESENTATION(#32808,#32933);
#32761=SHAPE_DEFINITION_REPRESENTATION(#32809,#32934);
#32762=SHAPE_DEFINITION_REPRESENTATION(#32810,#32935);
#32763=SHAPE_DEFINITION_REPRESENTATION(#32811,#32936);
#32764=SHAPE_DEFINITION_REPRESENTATION(#32812,#32937);
#32765=SHAPE_DEFINITION_REPRESENTATION(#32813,#32938);
#32766=SHAPE_DEFINITION_REPRESENTATION(#32814,#32939);
#32767=SHAPE_DEFINITION_REPRESENTATION(#32815,#32940);
#32768=SHAPE_DEFINITION_REPRESENTATION(#32816,#32941);
#32769=SHAPE_DEFINITION_REPRESENTATION(#32817,#32942);
#32770=SHAPE_DEFINITION_REPRESENTATION(#32818,#32943);
#32771=SHAPE_DEFINITION_REPRESENTATION(#32819,#32944);
#32772=SHAPE_DEFINITION_REPRESENTATION(#32820,#32945);
#32773=SHAPE_DEFINITION_REPRESENTATION(#32821,#32946);
#32774=SHAPE_DEFINITION_REPRESENTATION(#32822,#32947);
#32775=SHAPE_DEFINITION_REPRESENTATION(#32823,#32948);
#32776=SHAPE_DEFINITION_REPRESENTATION(#32824,#32949);
#32777=SHAPE_DEFINITION_REPRESENTATION(#32825,#32950);
#32778=SHAPE_DEFINITION_REPRESENTATION(#32826,#32951);
#32779=SHAPE_DEFINITION_REPRESENTATION(#32827,#32952);
#32780=SHAPE_DEFINITION_REPRESENTATION(#32833,#32953);
#32781=SHAPE_DEFINITION_REPRESENTATION(#32834,#32954);
#32782=SHAPE_DEFINITION_REPRESENTATION(#32835,#32955);
#32783=SHAPE_DEFINITION_REPRESENTATION(#32836,#32956);
#32784=SHAPE_DEFINITION_REPRESENTATION(#32837,#32957);
#32785=SHAPE_DEFINITION_REPRESENTATION(#32838,#32958);
#32786=SHAPE_DEFINITION_REPRESENTATION(#32843,#32959);
#32787=SHAPE_DEFINITION_REPRESENTATION(#32844,#32960);
#32788=SHAPE_DEFINITION_REPRESENTATION(#32845,#32961);
#32789=SHAPE_DEFINITION_REPRESENTATION(#32846,#32962);
#32790=SHAPE_DEFINITION_REPRESENTATION(#32847,#32963);
#32791=SHAPE_DEFINITION_REPRESENTATION(#32848,#32964);
#32792=SHAPE_DEFINITION_REPRESENTATION(#32849,#32965);
#32793=SHAPE_DEFINITION_REPRESENTATION(#32850,#32966);
#32794=SHAPE_DEFINITION_REPRESENTATION(#32851,#32967);
#32795=SHAPE_DEFINITION_REPRESENTATION(#32852,#32968);
#32796=SHAPE_DEFINITION_REPRESENTATION(#32853,#32969);
#32797=SHAPE_DEFINITION_REPRESENTATION(#32854,#32970);
#32798=SHAPE_DEFINITION_REPRESENTATION(#32855,#32971);
#32799=SHAPE_DEFINITION_REPRESENTATION(#32856,#32972);
#32800=SHAPE_DEFINITION_REPRESENTATION(#32857,#32973);
#32801=SHAPE_DEFINITION_REPRESENTATION(#32858,#32974);
#32802=SHAPE_DEFINITION_REPRESENTATION(#32922,#32975);
#32803=SHAPE_DEFINITION_REPRESENTATION(#32923,#32976);
#32804=PRODUCT_DEFINITION_SHAPE('',$,#32978);
#32805=PRODUCT_DEFINITION_SHAPE('',$,#32979);
#32806=PRODUCT_DEFINITION_SHAPE('',$,#32980);
#32807=PRODUCT_DEFINITION_SHAPE('',$,#32981);
#32808=PRODUCT_DEFINITION_SHAPE('',$,#32982);
#32809=PRODUCT_DEFINITION_SHAPE('',$,#32983);
#32810=PRODUCT_DEFINITION_SHAPE('',$,#32984);
#32811=PRODUCT_DEFINITION_SHAPE('',$,#32985);
#32812=PRODUCT_DEFINITION_SHAPE('',$,#32986);
#32813=PRODUCT_DEFINITION_SHAPE('',$,#32987);
#32814=PRODUCT_DEFINITION_SHAPE('',$,#32988);
#32815=PRODUCT_DEFINITION_SHAPE('',$,#32989);
#32816=PRODUCT_DEFINITION_SHAPE('',$,#32990);
#32817=PRODUCT_DEFINITION_SHAPE('',$,#32991);
#32818=PRODUCT_DEFINITION_SHAPE('',$,#32992);
#32819=PRODUCT_DEFINITION_SHAPE('',$,#32993);
#32820=PRODUCT_DEFINITION_SHAPE('',$,#32994);
#32821=PRODUCT_DEFINITION_SHAPE('',$,#32995);
#32822=PRODUCT_DEFINITION_SHAPE('',$,#32996);
#32823=PRODUCT_DEFINITION_SHAPE('',$,#32997);
#32824=PRODUCT_DEFINITION_SHAPE('',$,#32998);
#32825=PRODUCT_DEFINITION_SHAPE('',$,#32999);
#32826=PRODUCT_DEFINITION_SHAPE('',$,#33000);
#32827=PRODUCT_DEFINITION_SHAPE('',$,#33001);
#32828=PRODUCT_DEFINITION_SHAPE($,$,#362);
#32829=PRODUCT_DEFINITION_SHAPE($,$,#363);
#32830=PRODUCT_DEFINITION_SHAPE($,$,#364);
#32831=PRODUCT_DEFINITION_SHAPE($,$,#365);
#32832=PRODUCT_DEFINITION_SHAPE($,$,#366);
#32833=PRODUCT_DEFINITION_SHAPE('',$,#33002);
#32834=PRODUCT_DEFINITION_SHAPE('',$,#33003);
#32835=PRODUCT_DEFINITION_SHAPE('',$,#33004);
#32836=PRODUCT_DEFINITION_SHAPE('',$,#33005);
#32837=PRODUCT_DEFINITION_SHAPE('',$,#33006);
#32838=PRODUCT_DEFINITION_SHAPE('',$,#33007);
#32839=PRODUCT_DEFINITION_SHAPE($,$,#367);
#32840=PRODUCT_DEFINITION_SHAPE($,$,#368);
#32841=PRODUCT_DEFINITION_SHAPE($,$,#369);
#32842=PRODUCT_DEFINITION_SHAPE($,$,#370);
#32843=PRODUCT_DEFINITION_SHAPE('',$,#33008);
#32844=PRODUCT_DEFINITION_SHAPE('',$,#33009);
#32845=PRODUCT_DEFINITION_SHAPE('',$,#33010);
#32846=PRODUCT_DEFINITION_SHAPE('',$,#33011);
#32847=PRODUCT_DEFINITION_SHAPE('',$,#33012);
#32848=PRODUCT_DEFINITION_SHAPE('',$,#33013);
#32849=PRODUCT_DEFINITION_SHAPE('',$,#33014);
#32850=PRODUCT_DEFINITION_SHAPE('',$,#33015);
#32851=PRODUCT_DEFINITION_SHAPE('',$,#33016);
#32852=PRODUCT_DEFINITION_SHAPE('',$,#33017);
#32853=PRODUCT_DEFINITION_SHAPE('',$,#33018);
#32854=PRODUCT_DEFINITION_SHAPE('',$,#33019);
#32855=PRODUCT_DEFINITION_SHAPE('',$,#33020);
#32856=PRODUCT_DEFINITION_SHAPE('',$,#33021);
#32857=PRODUCT_DEFINITION_SHAPE('',$,#33022);
#32858=PRODUCT_DEFINITION_SHAPE('',$,#33023);
#32859=PRODUCT_DEFINITION_SHAPE($,$,#371);
#32860=PRODUCT_DEFINITION_SHAPE($,$,#372);
#32861=PRODUCT_DEFINITION_SHAPE($,$,#373);
#32862=PRODUCT_DEFINITION_SHAPE($,$,#374);
#32863=PRODUCT_DEFINITION_SHAPE($,$,#375);
#32864=PRODUCT_DEFINITION_SHAPE($,$,#376);
#32865=PRODUCT_DEFINITION_SHAPE($,$,#377);
#32866=PRODUCT_DEFINITION_SHAPE($,$,#378);
#32867=PRODUCT_DEFINITION_SHAPE($,$,#379);
#32868=PRODUCT_DEFINITION_SHAPE($,$,#380);
#32869=PRODUCT_DEFINITION_SHAPE($,$,#381);
#32870=PRODUCT_DEFINITION_SHAPE($,$,#382);
#32871=PRODUCT_DEFINITION_SHAPE($,$,#383);
#32872=PRODUCT_DEFINITION_SHAPE($,$,#384);
#32873=PRODUCT_DEFINITION_SHAPE($,$,#385);
#32874=PRODUCT_DEFINITION_SHAPE($,$,#386);
#32875=PRODUCT_DEFINITION_SHAPE($,$,#387);
#32876=PRODUCT_DEFINITION_SHAPE($,$,#388);
#32877=PRODUCT_DEFINITION_SHAPE($,$,#389);
#32878=PRODUCT_DEFINITION_SHAPE($,$,#390);
#32879=PRODUCT_DEFINITION_SHAPE($,$,#391);
#32880=PRODUCT_DEFINITION_SHAPE($,$,#392);
#32881=PRODUCT_DEFINITION_SHAPE($,$,#393);
#32882=PRODUCT_DEFINITION_SHAPE($,$,#394);
#32883=PRODUCT_DEFINITION_SHAPE($,$,#395);
#32884=PRODUCT_DEFINITION_SHAPE($,$,#396);
#32885=PRODUCT_DEFINITION_SHAPE($,$,#397);
#32886=PRODUCT_DEFINITION_SHAPE($,$,#398);
#32887=PRODUCT_DEFINITION_SHAPE($,$,#399);
#32888=PRODUCT_DEFINITION_SHAPE($,$,#400);
#32889=PRODUCT_DEFINITION_SHAPE($,$,#401);
#32890=PRODUCT_DEFINITION_SHAPE($,$,#402);
#32891=PRODUCT_DEFINITION_SHAPE($,$,#403);
#32892=PRODUCT_DEFINITION_SHAPE($,$,#404);
#32893=PRODUCT_DEFINITION_SHAPE($,$,#405);
#32894=PRODUCT_DEFINITION_SHAPE($,$,#406);
#32895=PRODUCT_DEFINITION_SHAPE($,$,#407);
#32896=PRODUCT_DEFINITION_SHAPE($,$,#408);
#32897=PRODUCT_DEFINITION_SHAPE($,$,#409);
#32898=PRODUCT_DEFINITION_SHAPE($,$,#410);
#32899=PRODUCT_DEFINITION_SHAPE($,$,#411);
#32900=PRODUCT_DEFINITION_SHAPE($,$,#412);
#32901=PRODUCT_DEFINITION_SHAPE($,$,#413);
#32902=PRODUCT_DEFINITION_SHAPE($,$,#414);
#32903=PRODUCT_DEFINITION_SHAPE($,$,#415);
#32904=PRODUCT_DEFINITION_SHAPE($,$,#416);
#32905=PRODUCT_DEFINITION_SHAPE($,$,#417);
#32906=PRODUCT_DEFINITION_SHAPE($,$,#418);
#32907=PRODUCT_DEFINITION_SHAPE($,$,#419);
#32908=PRODUCT_DEFINITION_SHAPE($,$,#420);
#32909=PRODUCT_DEFINITION_SHAPE($,$,#421);
#32910=PRODUCT_DEFINITION_SHAPE($,$,#422);
#32911=PRODUCT_DEFINITION_SHAPE($,$,#423);
#32912=PRODUCT_DEFINITION_SHAPE($,$,#424);
#32913=PRODUCT_DEFINITION_SHAPE($,$,#425);
#32914=PRODUCT_DEFINITION_SHAPE($,$,#426);
#32915=PRODUCT_DEFINITION_SHAPE($,$,#427);
#32916=PRODUCT_DEFINITION_SHAPE($,$,#428);
#32917=PRODUCT_DEFINITION_SHAPE($,$,#429);
#32918=PRODUCT_DEFINITION_SHAPE($,$,#430);
#32919=PRODUCT_DEFINITION_SHAPE($,$,#431);
#32920=PRODUCT_DEFINITION_SHAPE($,$,#432);
#32921=PRODUCT_DEFINITION_SHAPE($,$,#433);
#32922=PRODUCT_DEFINITION_SHAPE('',$,#33024);
#32923=PRODUCT_DEFINITION_SHAPE('',$,#33025);
#32924=PRODUCT_DEFINITION_SHAPE($,$,#434);
#32925=PRODUCT_DEFINITION_SHAPE($,$,#435);
#32926=PRODUCT_DEFINITION_SHAPE($,$,#436);
#32927=PRODUCT_DEFINITION_SHAPE($,$,#437);
#32928=PRODUCT_DEFINITION_SHAPE($,$,#438);
#32929=SHAPE_REPRESENTATION('',(#12999,#14151,#14152,#14153,#14154),#32703);
#32930=SHAPE_REPRESENTATION('',(#13000,#14077,#14078,#14079,#14080,#14081,
#14082,#14083,#14084,#14085,#14086,#14087,#14088,#14089,#14090,#14091,#14092,
#14093,#14094,#14095,#14096,#14097,#14098,#14099,#14100,#14101,#14102,#14103,
#14104,#14105,#14106,#14107,#14108,#14109,#14110,#14111,#14112,#14113,#14114,
#14115,#14116,#14117,#14118,#14119,#14120,#14121,#14122,#14123),#32704);
#32931=SHAPE_REPRESENTATION('',(#13001),#32705);
#32932=SHAPE_REPRESENTATION('',(#13038),#32706);
#32933=SHAPE_REPRESENTATION('',(#13045),#32707);
#32934=SHAPE_REPRESENTATION('',(#13052),#32708);
#32935=SHAPE_REPRESENTATION('',(#13122),#32709);
#32936=SHAPE_REPRESENTATION('',(#13139),#32710);
#32937=SHAPE_REPRESENTATION('',(#13160),#32711);
#32938=SHAPE_REPRESENTATION('',(#13177),#32712);
#32939=SHAPE_REPRESENTATION('',(#13198),#32713);
#32940=SHAPE_REPRESENTATION('',(#13218),#32714);
#32941=SHAPE_REPRESENTATION('',(#13253),#32715);
#32942=SHAPE_REPRESENTATION('',(#13278),#32716);
#32943=SHAPE_REPRESENTATION('',(#13303),#32717);
#32944=SHAPE_REPRESENTATION('',(#13338),#32718);
#32945=SHAPE_REPRESENTATION('',(#13363),#32719);
#32946=SHAPE_REPRESENTATION('',(#13388),#32720);
#32947=SHAPE_REPRESENTATION('',(#13414,#13537,#13538,#13539,#13540,#13541),
#32721);
#32948=SHAPE_REPRESENTATION('',(#13415),#32722);
#32949=SHAPE_REPRESENTATION('',(#13435),#32723);
#32950=SHAPE_REPRESENTATION('',(#13455),#32724);
#32951=SHAPE_REPRESENTATION('',(#13470),#32725);
#32952=SHAPE_REPRESENTATION('',(#13520),#32726);
#32953=SHAPE_REPRESENTATION('',(#13542),#32727);
#32954=SHAPE_REPRESENTATION('',(#13566,#13789,#13790,#13791,#13792),#32728);
#32955=SHAPE_REPRESENTATION('',(#13567),#32729);
#32956=SHAPE_REPRESENTATION('',(#13748),#32730);
#32957=SHAPE_REPRESENTATION('',(#13758),#32731);
#32958=SHAPE_REPRESENTATION('',(#13772),#32732);
#32959=SHAPE_REPRESENTATION('',(#13793,#14124,#14125,#14126,#14127,#14128,
#14129,#14130,#14131,#14132,#14133,#14134,#14135,#14136,#14137,#14138,#14139),
#32733);
#32960=SHAPE_REPRESENTATION('',(#13794),#32734);
#32961=SHAPE_REPRESENTATION('',(#13822),#32735);
#32962=SHAPE_REPRESENTATION('',(#13831),#32736);
#32963=SHAPE_REPRESENTATION('',(#13840),#32737);
#32964=SHAPE_REPRESENTATION('',(#13849),#32738);
#32965=SHAPE_REPRESENTATION('',(#13858),#32739);
#32966=SHAPE_REPRESENTATION('',(#13865),#32740);
#32967=SHAPE_REPRESENTATION('',(#13872),#32741);
#32968=SHAPE_REPRESENTATION('',(#13896),#32742);
#32969=SHAPE_REPRESENTATION('',(#13905),#32743);
#32970=SHAPE_REPRESENTATION('',(#13914),#32744);
#32971=SHAPE_REPRESENTATION('',(#13923),#32745);
#32972=SHAPE_REPRESENTATION('',(#14016),#32746);
#32973=SHAPE_REPRESENTATION('',(#14025),#32747);
#32974=SHAPE_REPRESENTATION('',(#14051),#32748);
#32975=SHAPE_REPRESENTATION('',(#14140,#14150),#32749);
#32976=SHAPE_REPRESENTATION('',(#14141),#32750);
#32977=PRODUCT_DEFINITION_CONTEXT('part definition',#33123,'design');
#32978=PRODUCT_DEFINITION('PAT-053','PAT-053',#33026,
#32977);
#32979=PRODUCT_DEFINITION('Press frame and guides',
'Press frame and guides',#33027,#32977);
#32980=PRODUCT_DEFINITION('Base','Base',#33028,#32977);
#32981=PRODUCT_DEFINITION('Foot strip','Foot strip',#33029,#32977);
#32982=PRODUCT_DEFINITION('Foot strip (1)','Foot strip (1)',#33030,#32977);
#32983=PRODUCT_DEFINITION('C frame','C frame',#33031,#32977);
#32984=PRODUCT_DEFINITION('Split ram guide','Split ram guide',#33032,#32977);
#32985=PRODUCT_DEFINITION('Guide keeper','Guide keeper',#33033,#32977);
#32986=PRODUCT_DEFINITION('Split ram guide (1)','Split ram guide (1)',#33034,
#32977);
#32987=PRODUCT_DEFINITION('Guide keeper (1)','Guide keeper (1)',#33035,#32977);
#32988=PRODUCT_DEFINITION('Anvil','Anvil',#33036,#32977);
#32989=PRODUCT_DEFINITION('Pinion bearing pedestal',
'Pinion bearing pedestal',#33037,#32977);
#32990=PRODUCT_DEFINITION('Pinion bearing cap','Pinion bearing cap',#33038,
#32977);
#32991=PRODUCT_DEFINITION('Pinion bearing cap (1)',
'Pinion bearing cap (1)',#33039,#32977);
#32992=PRODUCT_DEFINITION('Pinion bearing pedestal (1)',
'Pinion bearing pedestal (1)',#33040,#32977);
#32993=PRODUCT_DEFINITION('Pinion bearing cap (2)',
'Pinion bearing cap (2)',#33041,#32977);
#32994=PRODUCT_DEFINITION('Pinion bearing cap (3)',
'Pinion bearing cap (3)',#33042,#32977);
#32995=PRODUCT_DEFINITION('Cap Screw - M5x20','Cap Screw - M5x20',#33043,
#32977);
#32996=PRODUCT_DEFINITION('Sealed Ball Bearing - 12 x 32 x 10 mm',
'Sealed Ball Bearing - 12 x 32 x 10 mm',#33044,#32977);
#32997=PRODUCT_DEFINITION('Inner ring','Inner ring',#33045,#32977);
#32998=PRODUCT_DEFINITION('Outer ring','Outer ring',#33046,#32977);
#32999=PRODUCT_DEFINITION('Balls','Balls',#33047,#32977);
#33000=PRODUCT_DEFINITION('Cage','Cage',#33048,#32977);
#33001=PRODUCT_DEFINITION('Seals 2RS','Seals 2RS',#33049,#32977);
#33002=PRODUCT_DEFINITION('M4x10 Cap Screw','M4x10 Cap Screw',#33050,#32977);
#33003=PRODUCT_DEFINITION('Rack ram and pressure foot',
'Rack ram and pressure foot',#33051,#32977);
#33004=PRODUCT_DEFINITION('Rack ram','Rack ram',#33052,#32977);
#33005=PRODUCT_DEFINITION('Pressure foot','Pressure foot',#33053,#32977);
#33006=PRODUCT_DEFINITION('Upper travel collar','Upper travel collar',#33054,
#32977);
#33007=PRODUCT_DEFINITION('Socket Set Screw - M4x6',
'Socket Set Screw - M4x6',#33055,#32977);
#33008=PRODUCT_DEFINITION('Pinion and operating lever',
'Pinion and operating lever',#33056,#32977);
#33009=PRODUCT_DEFINITION('Pinion shaft','Pinion shaft',#33057,#32977);
#33010=PRODUCT_DEFINITION('Inner race spacer 20 mm',
'Inner race spacer 20 mm',#33058,#32977);
#33011=PRODUCT_DEFINITION('Inner race spacer 15 mm',
'Inner race spacer 15 mm',#33059,#32977);
#33012=PRODUCT_DEFINITION('Inner race spacer 3 mm',
'Inner race spacer 3 mm',#33060,#32977);
#33013=PRODUCT_DEFINITION('Inner race spacer 15 mm (1)',
'Inner race spacer 15 mm (1)',#33061,#32977);
#33014=PRODUCT_DEFINITION('Parallel key 4 x 4 x 14 mm',
'Parallel key 4 x 4 x 14 mm',#33062,#32977);
#33015=PRODUCT_DEFINITION('Parallel key 4 x 4 x 14 mm (1)',
'Parallel key 4 x 4 x 14 mm (1)',#33063,#32977);
#33016=PRODUCT_DEFINITION('Operating lever','Operating lever',#33064,#32977);
#33017=PRODUCT_DEFINITION('Handle sleeve','Handle sleeve',#33065,#32977);
#33018=PRODUCT_DEFINITION('Shaft keeper','Shaft keeper',#33066,#32977);
#33019=PRODUCT_DEFINITION('Shaft keeper (1)','Shaft keeper (1)',#33067,#32977);
#33020=PRODUCT_DEFINITION('Spur Gear - Module 2, 20 Teeth, 12 mm Bore',
'Spur Gear - Module 2, 20 Teeth, 12 mm Bore',#33068,#32977);
#33021=PRODUCT_DEFINITION('Flat Washer - M6','Flat Washer - M6',#33069,
#32977);
#33022=PRODUCT_DEFINITION('Cap Screw - M6x25','Cap Screw - M6x25',#33070,
#32977);
#33023=PRODUCT_DEFINITION('Cap Screw - M4x16','Cap Screw - M4x16',#33071,
#32977);
#33024=PRODUCT_DEFINITION('Revolving hand grip','Revolving hand grip',#33072,
#32977);
#33025=PRODUCT_DEFINITION('Revolving grip','Revolving grip',#33073,#32977);
#33026=PRODUCT_DEFINITION_FORMATION('',$,#33125);
#33027=PRODUCT_DEFINITION_FORMATION('',$,#33126);
#33028=PRODUCT_DEFINITION_FORMATION('',$,#33127);
#33029=PRODUCT_DEFINITION_FORMATION('',$,#33128);
#33030=PRODUCT_DEFINITION_FORMATION('',$,#33129);
#33031=PRODUCT_DEFINITION_FORMATION('',$,#33130);
#33032=PRODUCT_DEFINITION_FORMATION('',$,#33131);
#33033=PRODUCT_DEFINITION_FORMATION('',$,#33132);
#33034=PRODUCT_DEFINITION_FORMATION('',$,#33133);
#33035=PRODUCT_DEFINITION_FORMATION('',$,#33134);
#33036=PRODUCT_DEFINITION_FORMATION('',$,#33135);
#33037=PRODUCT_DEFINITION_FORMATION('',$,#33136);
#33038=PRODUCT_DEFINITION_FORMATION('',$,#33137);
#33039=PRODUCT_DEFINITION_FORMATION('',$,#33138);
#33040=PRODUCT_DEFINITION_FORMATION('',$,#33139);
#33041=PRODUCT_DEFINITION_FORMATION('',$,#33140);
#33042=PRODUCT_DEFINITION_FORMATION('',$,#33141);
#33043=PRODUCT_DEFINITION_FORMATION('',$,#33142);
#33044=PRODUCT_DEFINITION_FORMATION('',$,#33143);
#33045=PRODUCT_DEFINITION_FORMATION('',$,#33144);
#33046=PRODUCT_DEFINITION_FORMATION('',$,#33145);
#33047=PRODUCT_DEFINITION_FORMATION('',$,#33146);
#33048=PRODUCT_DEFINITION_FORMATION('',$,#33147);
#33049=PRODUCT_DEFINITION_FORMATION('',$,#33148);
#33050=PRODUCT_DEFINITION_FORMATION('',$,#33149);
#33051=PRODUCT_DEFINITION_FORMATION('',$,#33150);
#33052=PRODUCT_DEFINITION_FORMATION('',$,#33151);
#33053=PRODUCT_DEFINITION_FORMATION('',$,#33152);
#33054=PRODUCT_DEFINITION_FORMATION('',$,#33153);
#33055=PRODUCT_DEFINITION_FORMATION('',$,#33154);
#33056=PRODUCT_DEFINITION_FORMATION('',$,#33155);
#33057=PRODUCT_DEFINITION_FORMATION('',$,#33156);
#33058=PRODUCT_DEFINITION_FORMATION('',$,#33157);
#33059=PRODUCT_DEFINITION_FORMATION('',$,#33158);
#33060=PRODUCT_DEFINITION_FORMATION('',$,#33159);
#33061=PRODUCT_DEFINITION_FORMATION('',$,#33160);
#33062=PRODUCT_DEFINITION_FORMATION('',$,#33161);
#33063=PRODUCT_DEFINITION_FORMATION('',$,#33162);
#33064=PRODUCT_DEFINITION_FORMATION('',$,#33163);
#33065=PRODUCT_DEFINITION_FORMATION('',$,#33164);
#33066=PRODUCT_DEFINITION_FORMATION('',$,#33165);
#33067=PRODUCT_DEFINITION_FORMATION('',$,#33166);
#33068=PRODUCT_DEFINITION_FORMATION('',$,#33167);
#33069=PRODUCT_DEFINITION_FORMATION('',$,#33168);
#33070=PRODUCT_DEFINITION_FORMATION('',$,#33169);
#33071=PRODUCT_DEFINITION_FORMATION('',$,#33170);
#33072=PRODUCT_DEFINITION_FORMATION('',$,#33171);
#33073=PRODUCT_DEFINITION_FORMATION('',$,#33172);
#33074=PRODUCT_RELATED_PRODUCT_CATEGORY('PAT-053','PAT-053',(#33125));
#33075=PRODUCT_RELATED_PRODUCT_CATEGORY('Press frame and guides',
'Press frame and guides',(#33126));
#33076=PRODUCT_RELATED_PRODUCT_CATEGORY('Base','Base',(#33127));
#33077=PRODUCT_RELATED_PRODUCT_CATEGORY('Foot strip','Foot strip',(#33128));
#33078=PRODUCT_RELATED_PRODUCT_CATEGORY('Foot strip (1)',
'Foot strip (1)',(#33129));
#33079=PRODUCT_RELATED_PRODUCT_CATEGORY('C frame','C frame',(#33130));
#33080=PRODUCT_RELATED_PRODUCT_CATEGORY('Split ram guide',
'Split ram guide',(#33131));
#33081=PRODUCT_RELATED_PRODUCT_CATEGORY('Guide keeper','Guide keeper',(#33132));
#33082=PRODUCT_RELATED_PRODUCT_CATEGORY('Split ram guide (1)',
'Split ram guide (1)',(#33133));
#33083=PRODUCT_RELATED_PRODUCT_CATEGORY('Guide keeper (1)',
'Guide keeper (1)',(#33134));
#33084=PRODUCT_RELATED_PRODUCT_CATEGORY('Anvil','Anvil',(#33135));
#33085=PRODUCT_RELATED_PRODUCT_CATEGORY('Pinion bearing pedestal',
'Pinion bearing pedestal',(#33136));
#33086=PRODUCT_RELATED_PRODUCT_CATEGORY('Pinion bearing cap',
'Pinion bearing cap',(#33137));
#33087=PRODUCT_RELATED_PRODUCT_CATEGORY('Pinion bearing cap (1)',
'Pinion bearing cap (1)',(#33138));
#33088=PRODUCT_RELATED_PRODUCT_CATEGORY('Pinion bearing pedestal (1)',
'Pinion bearing pedestal (1)',(#33139));
#33089=PRODUCT_RELATED_PRODUCT_CATEGORY('Pinion bearing cap (2)',
'Pinion bearing cap (2)',(#33140));
#33090=PRODUCT_RELATED_PRODUCT_CATEGORY('Pinion bearing cap (3)',
'Pinion bearing cap (3)',(#33141));
#33091=PRODUCT_RELATED_PRODUCT_CATEGORY('Cap Screw - M5x20',
'Cap Screw - M5x20',(#33142));
#33092=PRODUCT_RELATED_PRODUCT_CATEGORY(
'Sealed Ball Bearing - 12 x 32 x 10 mm',
'Sealed Ball Bearing - 12 x 32 x 10 mm',(#33143));
#33093=PRODUCT_RELATED_PRODUCT_CATEGORY('Inner ring','Inner ring',(#33144));
#33094=PRODUCT_RELATED_PRODUCT_CATEGORY('Outer ring','Outer ring',(#33145));
#33095=PRODUCT_RELATED_PRODUCT_CATEGORY('Balls','Balls',(#33146));
#33096=PRODUCT_RELATED_PRODUCT_CATEGORY('Cage','Cage',(#33147));
#33097=PRODUCT_RELATED_PRODUCT_CATEGORY('Seals 2RS','Seals 2RS',(#33148));
#33098=PRODUCT_RELATED_PRODUCT_CATEGORY('M4x10 Cap Screw',
'M4x10 Cap Screw',(#33149));
#33099=PRODUCT_RELATED_PRODUCT_CATEGORY('Rack ram and pressure foot',
'Rack ram and pressure foot',(#33150));
#33100=PRODUCT_RELATED_PRODUCT_CATEGORY('Rack ram','Rack ram',(#33151));
#33101=PRODUCT_RELATED_PRODUCT_CATEGORY('Pressure foot','Pressure foot',
(#33152));
#33102=PRODUCT_RELATED_PRODUCT_CATEGORY('Upper travel collar',
'Upper travel collar',(#33153));
#33103=PRODUCT_RELATED_PRODUCT_CATEGORY('Socket Set Screw - M4x6',
'Socket Set Screw - M4x6',(#33154));
#33104=PRODUCT_RELATED_PRODUCT_CATEGORY('Pinion and operating lever',
'Pinion and operating lever',(#33155));
#33105=PRODUCT_RELATED_PRODUCT_CATEGORY('Pinion shaft','Pinion shaft',(#33156));
#33106=PRODUCT_RELATED_PRODUCT_CATEGORY('Inner race spacer 20 mm',
'Inner race spacer 20 mm',(#33157));
#33107=PRODUCT_RELATED_PRODUCT_CATEGORY('Inner race spacer 15 mm',
'Inner race spacer 15 mm',(#33158));
#33108=PRODUCT_RELATED_PRODUCT_CATEGORY('Inner race spacer 3 mm',
'Inner race spacer 3 mm',(#33159));
#33109=PRODUCT_RELATED_PRODUCT_CATEGORY('Inner race spacer 15 mm (1)',
'Inner race spacer 15 mm (1)',(#33160));
#33110=PRODUCT_RELATED_PRODUCT_CATEGORY('Parallel key 4 x 4 x 14 mm',
'Parallel key 4 x 4 x 14 mm',(#33161));
#33111=PRODUCT_RELATED_PRODUCT_CATEGORY(
'Parallel key 4 x 4 x 14 mm (1)','Parallel key 4 x 4 x 14 mm (1)',(#33162));
#33112=PRODUCT_RELATED_PRODUCT_CATEGORY('Operating lever',
'Operating lever',(#33163));
#33113=PRODUCT_RELATED_PRODUCT_CATEGORY('Handle sleeve','Handle sleeve',
(#33164));
#33114=PRODUCT_RELATED_PRODUCT_CATEGORY('Shaft keeper','Shaft keeper',(#33165));
#33115=PRODUCT_RELATED_PRODUCT_CATEGORY('Shaft keeper (1)',
'Shaft keeper (1)',(#33166));
#33116=PRODUCT_RELATED_PRODUCT_CATEGORY(
'Spur Gear - Module 2, 20 Teeth, 12 mm Bore',
'Spur Gear - Module 2, 20 Teeth, 12 mm Bore',(#33167));
#33117=PRODUCT_RELATED_PRODUCT_CATEGORY('Flat Washer - M6',
'Flat Washer - M6',(#33168));
#33118=PRODUCT_RELATED_PRODUCT_CATEGORY('Cap Screw - M6x25',
'Cap Screw - M6x25',(#33169));
#33119=PRODUCT_RELATED_PRODUCT_CATEGORY('Cap Screw - M4x16',
'Cap Screw - M4x16',(#33170));
#33120=PRODUCT_RELATED_PRODUCT_CATEGORY('Revolving hand grip',
'Revolving hand grip',(#33171));
#33121=PRODUCT_RELATED_PRODUCT_CATEGORY('Revolving grip',
'Revolving grip',(#33172));
#33122=APPLICATION_PROTOCOL_DEFINITION('international standard',
'automotive_design',2009,#33123);
#33123=APPLICATION_CONTEXT(
'Core Data for Automotive Mechanical Design Process');
#33124=PRODUCT_CONTEXT('part definition',#33123,'mechanical');
#33125=PRODUCT('PAT-053','PAT-053',
'PAT-053',(#33124));
#33126=PRODUCT('Press frame and guides','Press frame and guides',
'Press frame and guides',(#33124));
#33127=PRODUCT('Base','Base','Base',(#33124));
#33128=PRODUCT('Foot strip','Foot strip','Foot strip',(#33124));
#33129=PRODUCT('Foot strip (1)','Foot strip (1)','Foot strip (1)',(#33124));
#33130=PRODUCT('C frame','C frame','C frame',(#33124));
#33131=PRODUCT('Split ram guide','Split ram guide','Split ram guide',(#33124));
#33132=PRODUCT('Guide keeper','Guide keeper','Guide keeper',(#33124));
#33133=PRODUCT('Split ram guide (1)','Split ram guide (1)',
'Split ram guide (1)',(#33124));
#33134=PRODUCT('Guide keeper (1)','Guide keeper (1)','Guide keeper (1)',(#33124));
#33135=PRODUCT('Anvil','Anvil','Anvil',(#33124));
#33136=PRODUCT('Pinion bearing pedestal','Pinion bearing pedestal',
'Pinion bearing pedestal',(#33124));
#33137=PRODUCT('Pinion bearing cap','Pinion bearing cap',
'Pinion bearing cap',(#33124));
#33138=PRODUCT('Pinion bearing cap (1)','Pinion bearing cap (1)',
'Pinion bearing cap (1)',(#33124));
#33139=PRODUCT('Pinion bearing pedestal (1)',
'Pinion bearing pedestal (1)','Pinion bearing pedestal (1)',(#33124));
#33140=PRODUCT('Pinion bearing cap (2)','Pinion bearing cap (2)',
'Pinion bearing cap (2)',(#33124));
#33141=PRODUCT('Pinion bearing cap (3)','Pinion bearing cap (3)',
'Pinion bearing cap (3)',(#33124));
#33142=PRODUCT('Cap Screw - M5x20','Cap Screw - M5x20',
'Cap Screw - M5x20',(#33124));
#33143=PRODUCT('Sealed Ball Bearing - 12 x 32 x 10 mm',
'Sealed Ball Bearing - 12 x 32 x 10 mm',
'Sealed Ball Bearing - 12 x 32 x 10 mm',(#33124));
#33144=PRODUCT('Inner ring','Inner ring','Inner ring',(#33124));
#33145=PRODUCT('Outer ring','Outer ring','Outer ring',(#33124));
#33146=PRODUCT('Balls','Balls','Balls',(#33124));
#33147=PRODUCT('Cage','Cage','Cage',(#33124));
#33148=PRODUCT('Seals 2RS','Seals 2RS','Seals 2RS',(#33124));
#33149=PRODUCT('M4x10 Cap Screw','M4x10 Cap Screw','M4x10 Cap Screw',(#33124));
#33150=PRODUCT('Rack ram and pressure foot',
'Rack ram and pressure foot','Rack ram and pressure foot',(#33124));
#33151=PRODUCT('Rack ram','Rack ram','Rack ram',(#33124));
#33152=PRODUCT('Pressure foot','Pressure foot','Pressure foot',(#33124));
#33153=PRODUCT('Upper travel collar','Upper travel collar',
'Upper travel collar',(#33124));
#33154=PRODUCT('Socket Set Screw - M4x6','Socket Set Screw - M4x6',
'Socket Set Screw - M4x6',(#33124));
#33155=PRODUCT('Pinion and operating lever',
'Pinion and operating lever','Pinion and operating lever',(#33124));
#33156=PRODUCT('Pinion shaft','Pinion shaft','Pinion shaft',(#33124));
#33157=PRODUCT('Inner race spacer 20 mm','Inner race spacer 20 mm',
'Inner race spacer 20 mm',(#33124));
#33158=PRODUCT('Inner race spacer 15 mm','Inner race spacer 15 mm',
'Inner race spacer 15 mm',(#33124));
#33159=PRODUCT('Inner race spacer 3 mm','Inner race spacer 3 mm',
'Inner race spacer 3 mm',(#33124));
#33160=PRODUCT('Inner race spacer 15 mm (1)',
'Inner race spacer 15 mm (1)','Inner race spacer 15 mm (1)',(#33124));
#33161=PRODUCT('Parallel key 4 x 4 x 14 mm',
'Parallel key 4 x 4 x 14 mm','Parallel key 4 x 4 x 14 mm',(#33124));
#33162=PRODUCT('Parallel key 4 x 4 x 14 mm (1)',
'Parallel key 4 x 4 x 14 mm (1)','Parallel key 4 x 4 x 14 mm (1)',(#33124));
#33163=PRODUCT('Operating lever','Operating lever','Operating lever',(#33124));
#33164=PRODUCT('Handle sleeve','Handle sleeve','Handle sleeve',(#33124));
#33165=PRODUCT('Shaft keeper','Shaft keeper','Shaft keeper',(#33124));
#33166=PRODUCT('Shaft keeper (1)','Shaft keeper (1)','Shaft keeper (1)',(#33124));
#33167=PRODUCT('Spur Gear - Module 2, 20 Teeth, 12 mm Bore',
'Spur Gear - Module 2, 20 Teeth, 12 mm Bore',
'Spur Gear - Module 2, 20 Teeth, 12 mm Bore',(#33124));
#33168=PRODUCT('Flat Washer - M6','Flat Washer - M6','Flat Washer - M6',
(#33124));
#33169=PRODUCT('Cap Screw - M6x25','Cap Screw - M6x25',
'Cap Screw - M6x25',(#33124));
#33170=PRODUCT('Cap Screw - M4x16','Cap Screw - M4x16',
'Cap Screw - M4x16',(#33124));
#33171=PRODUCT('Revolving hand grip','Revolving hand grip',
'Revolving hand grip',(#33124));
#33172=PRODUCT('Revolving grip','Revolving grip','Revolving grip',(#33124));
#33173=PRESENTATION_STYLE_ASSIGNMENT((#33179));
#33174=PRESENTATION_STYLE_ASSIGNMENT((#33180));
#33175=PRESENTATION_STYLE_ASSIGNMENT((#33181));
#33176=PRESENTATION_STYLE_ASSIGNMENT((#33182));
#33177=PRESENTATION_STYLE_ASSIGNMENT((#33183));
#33178=PRESENTATION_STYLE_ASSIGNMENT((#33184));
#33179=SURFACE_STYLE_USAGE(.BOTH.,#33185);
#33180=SURFACE_STYLE_USAGE(.BOTH.,#33186);
#33181=SURFACE_STYLE_USAGE(.BOTH.,#33187);
#33182=SURFACE_STYLE_USAGE(.BOTH.,#33188);
#33183=SURFACE_STYLE_USAGE(.BOTH.,#33189);
#33184=SURFACE_STYLE_USAGE(.BOTH.,#33190);
#33185=SURFACE_SIDE_STYLE('',(#33191));
#33186=SURFACE_SIDE_STYLE('',(#33192));
#33187=SURFACE_SIDE_STYLE('',(#33193));
#33188=SURFACE_SIDE_STYLE('',(#33194));
#33189=SURFACE_SIDE_STYLE('',(#33195));
#33190=SURFACE_SIDE_STYLE('',(#33196));
#33191=SURFACE_STYLE_FILL_AREA(#33197);
#33192=SURFACE_STYLE_FILL_AREA(#33198);
#33193=SURFACE_STYLE_FILL_AREA(#33199);
#33194=SURFACE_STYLE_FILL_AREA(#33200);
#33195=SURFACE_STYLE_FILL_AREA(#33201);
#33196=SURFACE_STYLE_FILL_AREA(#33202);
#33197=FILL_AREA_STYLE('Steel - Satin',(#33203));
#33198=FILL_AREA_STYLE('CAD Library Painted - Deep blue',(#33204));
#33199=FILL_AREA_STYLE('CAD Library Painted - Engineering blue',(#33205));
#33200=FILL_AREA_STYLE('CAD Library Painted - Steel gray',(#33206));
#33201=FILL_AREA_STYLE('CAD Library Painted - Graphite',(#33207));
#33202=FILL_AREA_STYLE('CAD Library Painted - Light blue',(#33208));
#33203=FILL_AREA_STYLE_COLOUR('Steel - Satin',#33209);
#33204=FILL_AREA_STYLE_COLOUR('CAD Library Painted - Deep blue',#33210);
#33205=FILL_AREA_STYLE_COLOUR('CAD Library Painted - Engineering blue',
#33211);
#33206=FILL_AREA_STYLE_COLOUR('CAD Library Painted - Steel gray',#33212);
#33207=FILL_AREA_STYLE_COLOUR('CAD Library Painted - Graphite',#33213);
#33208=FILL_AREA_STYLE_COLOUR('CAD Library Painted - Light blue',#33214);
#33209=COLOUR_RGB('Steel - Satin',0.627450980392157,0.627450980392157,0.627450980392157);
#33210=COLOUR_RGB('CAD Library Painted - Deep blue',0.0784313725490196,
0.203921568627451,0.349019607843137);
#33211=COLOUR_RGB('CAD Library Painted - Engineering blue',0.12156862745098,
0.356862745098039,0.6);
#33212=COLOUR_RGB('CAD Library Painted - Steel gray',0.592156862745098,
0.631372549019608,0.67843137254902);
#33213=COLOUR_RGB('CAD Library Painted - Graphite',0.168627450980392,0.192156862745098,
0.231372549019608);
#33214=COLOUR_RGB('CAD Library Painted - Light blue',0.286274509803922,
0.552941176470588,0.780392156862745);
#33215=COLOUR_RGB('Dark Blue',0.08,0.2,0.34);
#33216=FILL_AREA_STYLE_COLOUR('',#33215);
#33217=FILL_AREA_STYLE('',(#33216));
#33218=SURFACE_STYLE_FILL_AREA(#33217);
#33219=SURFACE_SIDE_STYLE('',(#33218));
#33220=SURFACE_STYLE_USAGE(.BOTH.,#33219);
#33221=PRESENTATION_STYLE_ASSIGNMENT((#33220));
#33222=COLOUR_RGB('Light Blue',0.38,0.62,0.78);
#33223=FILL_AREA_STYLE_COLOUR('',#33222);
#33224=FILL_AREA_STYLE('',(#33223));
#33225=SURFACE_STYLE_FILL_AREA(#33224);
#33226=SURFACE_SIDE_STYLE('',(#33225));
#33227=SURFACE_STYLE_USAGE(.BOTH.,#33226);
#33228=PRESENTATION_STYLE_ASSIGNMENT((#33227));
#33229=COLOUR_RGB('Sky Blue',0.24,0.69,0.87);
#33230=FILL_AREA_STYLE_COLOUR('',#33229);
#33231=FILL_AREA_STYLE('',(#33230));
#33232=SURFACE_STYLE_FILL_AREA(#33231);
#33233=SURFACE_SIDE_STYLE('',(#33232));
#33234=SURFACE_STYLE_USAGE(.BOTH.,#33233);
#33235=PRESENTATION_STYLE_ASSIGNMENT((#33234));
#33236=COLOUR_RGB('Grey',0.48,0.52,0.57);
#33237=FILL_AREA_STYLE_COLOUR('',#33236);
#33238=FILL_AREA_STYLE('',(#33237));
#33239=SURFACE_STYLE_FILL_AREA(#33238);
#33240=SURFACE_SIDE_STYLE('',(#33239));
#33241=SURFACE_STYLE_USAGE(.BOTH.,#33240);
#33242=PRESENTATION_STYLE_ASSIGNMENT((#33241));
#33243=COLOUR_RGB('Black',0.12,0.14,0.17);
#33244=FILL_AREA_STYLE_COLOUR('',#33243);
#33245=FILL_AREA_STYLE('',(#33244));
#33246=SURFACE_STYLE_FILL_AREA(#33245);
#33247=SURFACE_SIDE_STYLE('',(#33246));
#33248=SURFACE_STYLE_USAGE(.BOTH.,#33247);
#33249=PRESENTATION_STYLE_ASSIGNMENT((#33248));
#33250=COLOUR_RGB('Off White',0.89,0.88,0.83);
#33251=FILL_AREA_STYLE_COLOUR('',#33250);
#33252=FILL_AREA_STYLE('',(#33251));
#33253=SURFACE_STYLE_FILL_AREA(#33252);
#33254=SURFACE_SIDE_STYLE('',(#33253));
#33255=SURFACE_STYLE_USAGE(.BOTH.,#33254);
#33256=PRESENTATION_STYLE_ASSIGNMENT((#33255));
ENDSEC;
END-ISO-10303-21;
